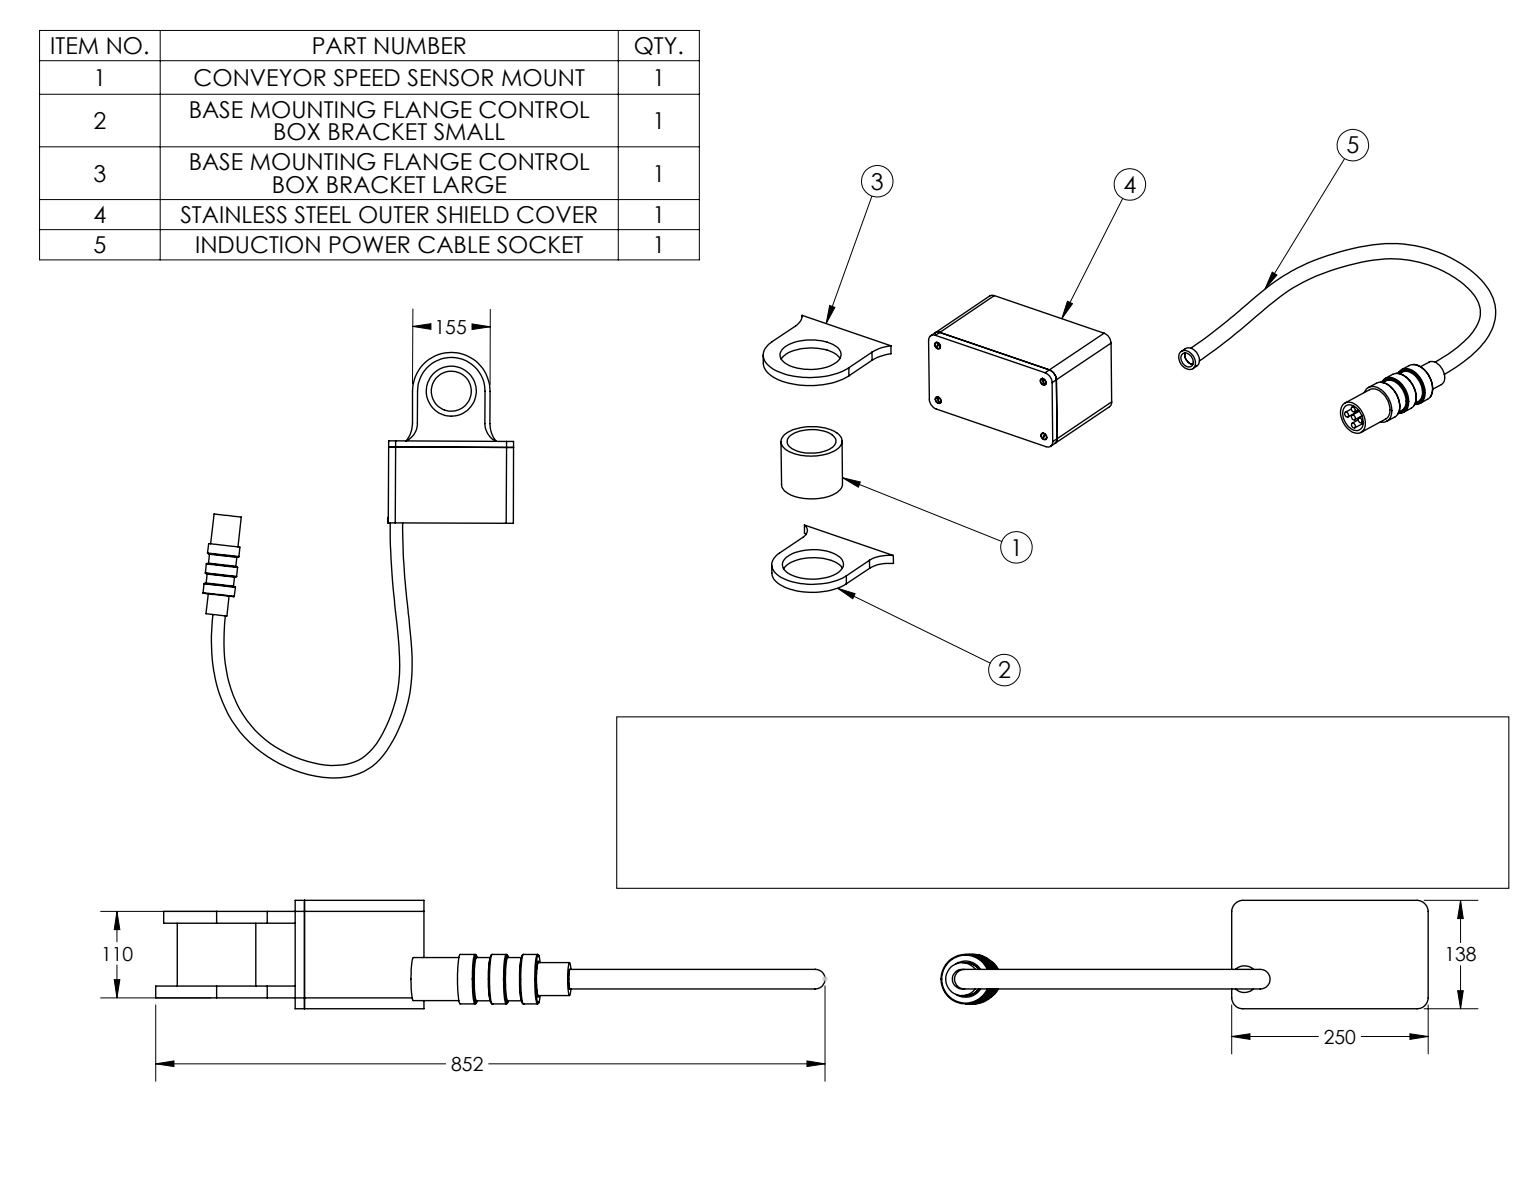
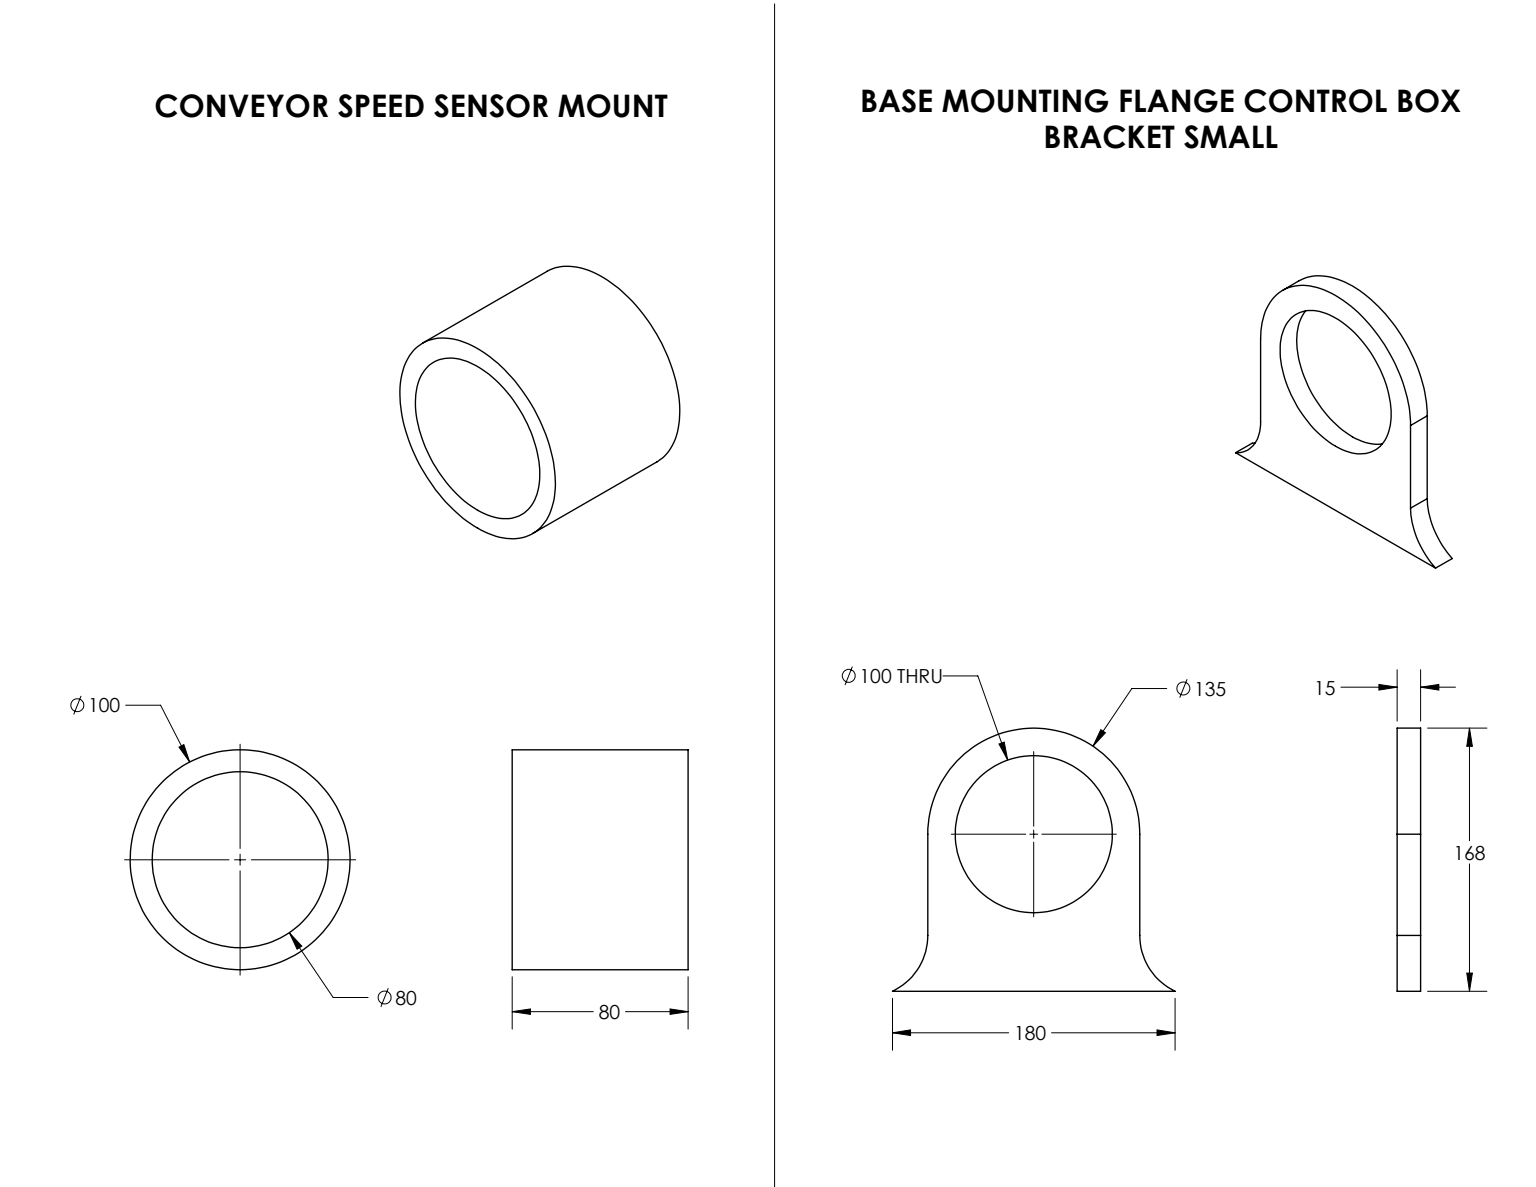
ISO-10303-21;
HEADER;
FILE_DESCRIPTION (('STEP AP214'),
    '1' );
FILE_NAME ('MAT-023',
    '2026-10-28T18:30:06',
    ( '' ),
    ( '' ),
    'SwSTEP 2.0',
    'SolidWorks 2024',
    '' );
FILE_SCHEMA (( 'AUTOMOTIVE_DESIGN' ));
ENDSEC;

DATA;
#1 = CARTESIAN_POINT ( 'NONE',  ( -382.0077566144223624, 5.421010862429173848E-17, 175.3290427019271078 ) ) ;
#2 = ORIENTED_EDGE ( 'NONE', *, *, #5398, .F. ) ;
#3 = APPLICATION_CONTEXT ( 'automotive_design' ) ;
#4 = DIRECTION ( 'NONE',  ( 5.551115123125772841E-17, -1.848892746611743135E-31, -1.000000000000000000 ) ) ;
#5 = DIRECTION ( 'NONE',  ( -0.9955873536034884896, 5.465719896581968711E-31, -0.09383933793885443353 ) ) ;
#6 = CARTESIAN_POINT ( 'NONE',  ( -84.02857808274397655, 98.45434506795682239, 152.0000000000000853 ) ) ;
#7 = DIRECTION ( 'NONE',  ( -0.000000000000000000, -1.000000000000000000, -0.000000000000000000 ) ) ;
#8 = VERTEX_POINT ( 'NONE', #1404 ) ;
#9 = ORIENTED_EDGE ( 'NONE', *, *, #3496, .F. ) ;
#10 = DIRECTION ( 'NONE',  ( 0.4205749795070160557, -0.9072577839912276954, -5.551115123125780853E-17 ) ) ;
#11 = CARTESIAN_POINT ( 'NONE',  ( 0.000000000000000000, 0.000000000000000000, 0.000000000000000000 ) ) ;
#12 = DIRECTION ( 'NONE',  ( -0.09383933793885568253, 2.673190762809473730E-31, 0.9955873536034882676 ) ) ;
#13 = EDGE_CURVE ( 'NONE', #832, #1072, #4200, .T. ) ;
#14 = SURFACE_SIDE_STYLE ('',( #2418 ) ) ;
#15 = VECTOR ( 'NONE', #512, 1000.000000000000000 ) ;
#16 = CARTESIAN_POINT ( 'NONE',  ( 29.23877717791895492, 0.000000000000000000, 67.09613410133256650 ) ) ;
#17 = CARTESIAN_POINT ( 'NONE',  ( -86.97194166595129161, 3.740497495074990297E-15, 531.0655262460708173 ) ) ;
#18 = CARTESIAN_POINT ( 'NONE',  ( -367.0460729392618759, 0.000000000000000000, 268.0688838304710089 ) ) ;
#19 = AXIS2_PLACEMENT_3D ( 'NONE', #2675, #4355, #3941 ) ;
#20 = ORIENTED_EDGE ( 'NONE', *, *, #2616, .F. ) ;
#21 = VECTOR ( 'NONE', #4832, 999.9999999999998863 ) ;
#22 = ORIENTED_EDGE ( 'NONE', *, *, #960, .T. ) ;
#23 = CARTESIAN_POINT ( 'NONE',  ( -84.02857808274400497, -39.54565493204319182, -5.551115123125782702E-14 ) ) ;
#24 = CIRCLE ( 'NONE', #2310, 4.382543221487789964 ) ;
#25 = AXIS2_PLACEMENT_3D ( 'NONE', #1773, #1368, #5093 ) ;
#26 = ORIENTED_EDGE ( 'NONE', *, *, #5308, .T. ) ;
#27 = DIRECTION ( 'NONE',  ( -1.000000000000000000, 0.000000000000000000, -7.228014483236656373E-17 ) ) ;
#28 = VECTOR ( 'NONE', #1957, 1000.000000000000114 ) ;
#29 = CIRCLE ( 'NONE', #5298, 39.24395386344908587 ) ;
#30 = DIRECTION ( 'NONE',  ( 0.09383933793885537722, -2.626968444144180508E-31, -0.9955873536034883786 ) ) ;
#31 = DIRECTION ( 'NONE',  ( 0.000000000000000000, 1.000000000000000000, 0.000000000000000000 ) ) ;
#32 = DIRECTION ( 'NONE',  ( 0.09383933793885537722, -2.626968444144180508E-31, -0.9955873536034883786 ) ) ;
#33 = DIRECTION ( 'NONE',  ( 1.000000000000000000, 0.000000000000000000, 0.000000000000000000 ) ) ;
#34 = CARTESIAN_POINT ( 'NONE',  ( -346.0119820531829191, 0.000000000000000000, 118.4559012928527721 ) ) ;
#35 = CIRCLE ( 'NONE', #3119, 30.50000000000124345 ) ;
#36 = AXIS2_PLACEMENT_3D ( 'NONE', #3078, #3164, #1374 ) ;
#37 = AXIS2_PLACEMENT_3D ( 'NONE', #784, #1656, #4559 ) ;
#38 = ORIENTED_EDGE ( 'NONE', *, *, #4267, .T. ) ;
#39 = ORIENTED_EDGE ( 'NONE', *, *, #4059, .T. ) ;
#40 = EDGE_LOOP ( 'NONE', ( #5035, #3170, #2808, #3510 ) ) ;
#41 = DIRECTION ( 'NONE',  ( -1.000000000000000000, 0.000000000000000000, 0.000000000000000000 ) ) ;
#42 = AXIS2_PLACEMENT_3D ( 'NONE', #2101, #4638, #4224 ) ;
#43 = DIRECTION ( 'NONE',  ( 0.9955873536034884896, -5.462637660443545995E-31, 0.09383933793885503027 ) ) ;
#44 = CARTESIAN_POINT ( 'NONE',  ( -379.2497704504713738, 6.080251870909620328E-15, 135.4117092198481487 ) ) ;
#45 = PRODUCT_DEFINITION_SHAPE ( 'NONE', 'NONE',  #5437 ) ;
#46 = CYLINDRICAL_SURFACE ( 'NONE', #25, 6.000000000000032863 ) ;
#47 = EDGE_LOOP ( 'NONE', ( #4656, #3822, #3045, #5223 ) ) ;
#48 = DIRECTION ( 'NONE',  ( 0.09383933793885568253, -2.673190762809473730E-31, -0.9955873536034882676 ) ) ;
#49 = CARTESIAN_POINT ( 'NONE',  ( 6.585909452853061730, 3.740497495074990297E-15, 393.9228865916071527 ) ) ;
#50 = CARTESIAN_POINT ( 'NONE',  ( -74.77857808274409024, -21.54565493204320248, -26.84924240491759662 ) ) ;
#51 = ORIENTED_EDGE ( 'NONE', *, *, #5105, .T. ) ;
#52 = ORIENTED_EDGE ( 'NONE', *, *, #5333, .F. ) ;
#53 = CARTESIAN_POINT ( 'NONE',  ( -60.76122282208098824, 0.000000000000000000, 167.0961341013325523 ) ) ;
#54 = SHAPE_REPRESENTATION_RELATIONSHIP ( 'NONE' , 'NONE' ,  #825, #4179 ) ;
#55 = FACE_BOUND ( 'NONE', #4165, .T. ) ;
#56 = EDGE_CURVE ( 'NONE', #1665, #3075, #3058, .T. ) ;
#57 = EDGE_CURVE ( 'NONE', #2668, #1622, #1040, .T. ) ;
#58 = ORIENTED_EDGE ( 'NONE', *, *, #3746, .T. ) ;
#59 = PLANE ( 'NONE',  #568 ) ;
#60 = ADVANCED_FACE ( 'NONE', ( #4394, #2277 ), #4750, .F. ) ;
#61 = EDGE_CURVE ( 'NONE', #167, #979, #3936, .T. ) ;
#62 = CARTESIAN_POINT ( 'NONE',  ( -84.02857808274400497, -39.54565493204319893, -11.99999999999984368 ) ) ;
#63 = CARTESIAN_POINT ( 'NONE',  ( 11.81831109762766729, -25.00000000000000355, 46.95220429669349471 ) ) ;
#64 = SURFACE_STYLE_USAGE ( .BOTH. , #1323 ) ;
#65 = DIRECTION ( 'NONE',  ( -1.000000000000000000, 0.000000000000000000, 0.000000000000000000 ) ) ;
#66 = CARTESIAN_POINT ( 'NONE',  ( 133.9714219172562366, -21.54565493204323090, -9.999999999999841904 ) ) ;
#67 = ORIENTED_EDGE ( 'NONE', *, *, #2103, .T. ) ;
#68 = ORIENTED_EDGE ( 'NONE', *, *, #1541, .F. ) ;
#69 = ORIENTED_EDGE ( 'NONE', *, *, #2616, .T. ) ;
#70 = DIRECTION ( 'NONE',  ( 0.09383933793885537722, -2.626968444144180508E-31, -0.9955873536034883786 ) ) ;
#71 = CARTESIAN_POINT ( 'NONE',  ( -13.34676807733242754, 3.807633061153780218E-15, 36.33529372355719289 ) ) ;
#72 = CARTESIAN_POINT ( 'NONE',  ( -84.02857808274397655, 98.45434506795682239, 152.0000000000000853 ) ) ;
#73 = CARTESIAN_POINT ( 'NONE',  ( -98.02857808274420393, -25.54565493204307813, 152.0000000000001990 ) ) ;
#74 = ORIENTED_EDGE ( 'NONE', *, *, #1802, .F. ) ;
#75 = CARTESIAN_POINT ( 'NONE',  ( -299.8611223228758149, 3.740497495074990297E-15, 439.6443911606511392 ) ) ;
#76 = CARTESIAN_POINT ( 'NONE',  ( -80.59222536594943165, -24.99999999999981881, 529.1597157429057461 ) ) ;
#77 = CARTESIAN_POINT ( 'NONE',  ( -84.02857808274407603, 84.45434506795682239, -11.99999999999995559 ) ) ;
#78 = EDGE_CURVE ( 'NONE', #3915, #4669, #546, .T. ) ;
#79 = ORIENTED_EDGE ( 'NONE', *, *, #2485, .T. ) ;
#80 = ORIENTED_EDGE ( 'NONE', *, *, #160, .F. ) ;
#81 = LINE ( 'NONE', #5048, #3867 ) ;
#82 = ORIENTED_EDGE ( 'NONE', *, *, #2341, .F. ) ;
#83 = CARTESIAN_POINT ( 'NONE',  ( -30.63277980166695258, 0.000000000000000000, 527.1358351633697339 ) ) ;
#84 = ORIENTED_EDGE ( 'NONE', *, *, #1033, .T. ) ;
#85 = EDGE_CURVE ( 'NONE', #3013, #195, #2089, .T. ) ;
#86 = PLANE ( 'NONE',  #1169 ) ;
#87 = CARTESIAN_POINT ( 'NONE',  ( -198.3455225866221667, -25.00000000000003197, 518.3576047634796851 ) ) ;
#88 = CARTESIAN_POINT ( 'NONE',  ( -72.60637664584184847, 3.252606517456513302E-16, 552.9197695054128872 ) ) ;
#89 = CARTESIAN_POINT ( 'NONE',  ( 151.9714219172562935, -25.54565493204309234, -5.551115123125782702E-14 ) ) ;
#90 = ADVANCED_FACE ( 'NONE', ( #1835, #4370 ), #3525, .T. ) ;
#91 = EDGE_LOOP ( 'NONE', ( #1303, #4558, #3690, #426 ) ) ;
#92 = ORIENTED_EDGE ( 'NONE', *, *, #2910, .T. ) ;
#93 = ORIENTED_EDGE ( 'NONE', *, *, #1802, .T. ) ;
#94 = CARTESIAN_POINT ( 'NONE',  ( -328.0684036055322963, 2.759321206427281912E-15, 40.79703369235946298 ) ) ;
#95 = FACE_OUTER_BOUND ( 'NONE', #4381, .T. ) ;
#96 = DIRECTION ( 'NONE',  ( 5.551115123125772841E-17, -1.848892746611743135E-31, -1.000000000000000000 ) ) ;
#97 = CYLINDRICAL_SURFACE ( 'NONE', #5382, 27.43532828739476415 ) ;
#98 = ORIENTED_EDGE ( 'NONE', *, *, #2578, .T. ) ;
#99 = FACE_OUTER_BOUND ( 'NONE', #532, .T. ) ;
#100 = CARTESIAN_POINT ( 'NONE',  ( -16.96312831416361533, -24.99999999999981881, 463.2830513152442222 ) ) ;
#101 = DIRECTION ( 'NONE',  ( 0.09383933793885568253, -2.673190762809473730E-31, -0.9955873536034882676 ) ) ;
#102 = AXIS2_PLACEMENT_3D ( 'NONE', #3097, #2631, #4309 ) ;
#103 = ORIENTED_EDGE ( 'NONE', *, *, #5162, .T. ) ;
#104 = AXIS2_PLACEMENT_3D ( 'NONE', #682, #917, #4326 ) ;
#105 = CARTESIAN_POINT ( 'NONE',  ( 29.23877717791895492, -14.99999999999998579, 67.09613410133256650 ) ) ;
#106 = LINE ( 'NONE', #1784, #5082 ) ;
#107 =( NAMED_UNIT ( * ) PLANE_ANGLE_UNIT ( ) SI_UNIT ( $, .RADIAN. ) );
#108 = AXIS2_PLACEMENT_3D ( 'NONE', #5417, #1651, #2776 ) ;
#109 = EDGE_LOOP ( 'NONE', ( #1428, #2018, #1351, #4648 ) ) ;
#110 = CARTESIAN_POINT ( 'NONE',  ( -285.5643670724598451, 2.222614453595284090E-15, 494.2304181244439292 ) ) ;
#111 = EDGE_CURVE ( 'NONE', #1596, #1814, #592, .T. ) ;
#112 = DIRECTION ( 'NONE',  ( 5.551115123125772841E-17, -1.848892746611743135E-31, -1.000000000000000000 ) ) ;
#113 = CARTESIAN_POINT ( 'NONE',  ( -336.1069982926118769, 1.517883041479706208E-15, 349.6877309229317916 ) ) ;
#114 = AXIS2_PLACEMENT_3D ( 'NONE', #1904, #666, #4466 ) ;
#115 = CARTESIAN_POINT ( 'NONE',  ( -364.1439395362590972, 2.398458366376004494E-13, 237.2787335496881553 ) ) ;
#116 = CARTESIAN_POINT ( 'NONE',  ( 127.9714219172562224, -21.54565493204319182, -2.000000000000002220 ) ) ;
#117 = CIRCLE ( 'NONE', #1187, 31.50000000000125766 ) ;
#118 = ORIENTED_EDGE ( 'NONE', *, *, #13, .F. ) ;
#119 = ORIENTED_EDGE ( 'NONE', *, *, #3733, .F. ) ;
#120 = ORIENTED_EDGE ( 'NONE', *, *, #4299, .T. ) ;
#121 = DIRECTION ( 'NONE',  ( 0.9998833722232041143, -6.898681060795032408E-31, -0.01527226085271977431 ) ) ;
#122 = LINE ( 'NONE', #1849, #2478 ) ;
#123 = CARTESIAN_POINT ( 'NONE',  ( 29.23877717791899400, 15.00000000000001421, -10.40386589866737488 ) ) ;
#124 = MECHANICAL_DESIGN_GEOMETRIC_PRESENTATION_REPRESENTATION (  '', ( #1085 ), #3988 ) ;
#125 = AXIS2_PLACEMENT_3D ( 'NONE', #1233, #2528, #573 ) ;
#126 = AXIS2_PLACEMENT_3D ( 'NONE', #266, #1941, #351 ) ;
#127 = SURFACE_STYLE_FILL_AREA ( #3020 ) ;
#128 = ORIENTED_EDGE ( 'NONE', *, *, #2251, .T. ) ;
#129 = EDGE_CURVE ( 'NONE', #2973, #1648, #4118, .T. ) ;
#130 = EDGE_CURVE ( 'NONE', #8, #1142, #2447, .T. ) ;
#131 = AXIS2_PLACEMENT_3D ( 'NONE', #4848, #2356, #4561 ) ;
#132 = AXIS2_PLACEMENT_3D ( 'NONE', #1581, #2880, #843 ) ;
#133 = CARTESIAN_POINT ( 'NONE',  ( 136.6230329513293213, 75.92317977368846016, -10.00000000000006395 ) ) ;
#134 = CARTESIAN_POINT ( 'NONE',  ( 23.50217280487988347, -24.99999999999981881, 428.9062724124379997 ) ) ;
#135 = CARTESIAN_POINT ( 'NONE',  ( -77.37696704867106234, 84.98551036222526989, -9.999999999999953815 ) ) ;
#136 = DIRECTION ( 'NONE',  ( -0.09383933793885536334, 2.611561004589082183E-31, 0.9955873536034882676 ) ) ;
#137 = CARTESIAN_POINT ( 'NONE',  ( -49.96441683051505578, 2.222614453595284090E-15, 542.4422122871075089 ) ) ;
#138 = DIRECTION ( 'NONE',  ( 0.3430150920801929848, -4.307264849556244242E-30, 0.9393298923196350403 ) ) ;
#139 = ORIENTED_EDGE ( 'NONE', *, *, #3662, .F. ) ;
#140 = CARTESIAN_POINT ( 'NONE',  ( -334.2906958041416488, 0.000000000000000000, 430.9840019716568804 ) ) ;
#141 = EDGE_LOOP ( 'NONE', ( #309, #4866, #1878, #776 ) ) ;
#142 = FACE_OUTER_BOUND ( 'NONE', #4109, .T. ) ;
#143 = DIRECTION ( 'NONE',  ( -5.551115123125772841E-17, 1.848892746611743135E-31, 1.000000000000000000 ) ) ;
#144 = CIRCLE ( 'NONE', #4108, 28.50000000000127898 ) ;
#145 = DIRECTION ( 'NONE',  ( 5.551115123125772841E-17, -1.848892746611743135E-31, -1.000000000000000000 ) ) ;
#146 = ORIENTED_EDGE ( 'NONE', *, *, #3858, .T. ) ;
#147 = ORIENTED_EDGE ( 'NONE', *, *, #2271, .F. ) ;
#148 = CARTESIAN_POINT ( 'NONE',  ( 29.23877717791895492, -14.99999999999998579, 117.0961341013325665 ) ) ;
#149 = CARTESIAN_POINT ( 'NONE',  ( -0.8482259245422840710, 2.276824562219559311E-15, 36.14439046289818691 ) ) ;
#150 = CARTESIAN_POINT ( 'NONE',  ( 132.2270686671744500, 85.40608534173220789, -11.99999999999990052 ) ) ;
#151 =( NAMED_UNIT ( * ) PLANE_ANGLE_UNIT ( ) SI_UNIT ( $, .RADIAN. ) );
#152 = ORIENTED_EDGE ( 'NONE', *, *, #1132, .F. ) ;
#153 = VECTOR ( 'NONE', #3723, 1000.000000000000000 ) ;
#154 = CIRCLE ( 'NONE', #4288, 50.00000000000000000 ) ;
#155 = DIRECTION ( 'NONE',  ( 0.01527226085271972227, 2.095411779493299033E-31, 0.9998833722232041143 ) ) ;
#156 = EDGE_CURVE ( 'NONE', #4669, #533, #2181, .T. ) ;
#157 = CARTESIAN_POINT ( 'NONE',  ( -57.28677601057306390, -24.99999999999981881, 546.4981013186294376 ) ) ;
#158 = CARTESIAN_POINT ( 'NONE',  ( -314.5571410767332736, 5.421010862426289575E-17, 120.4162530843239978 ) ) ;
#159 = EDGE_CURVE ( 'NONE', #2587, #907, #154, .T. ) ;
#160 = EDGE_CURVE ( 'NONE', #4568, #5281, #4983, .T. ) ;
#161 = ADVANCED_FACE ( 'NONE', ( #1208 ), #3224, .T. ) ;
#162 = EDGE_LOOP ( 'NONE', ( #316, #3364, #1642, #4137 ) ) ;
#163 = AXIS2_PLACEMENT_3D ( 'NONE', #847, #4231, #4697 ) ;
#164 = CARTESIAN_POINT ( 'NONE',  ( -364.1439395362591540, 2.222614453595284090E-15, 237.2787335496894343 ) ) ;
#165 =( NAMED_UNIT ( * ) SI_UNIT ( $, .STERADIAN. ) SOLID_ANGLE_UNIT ( ) );
#166 = EDGE_CURVE ( 'NONE', #533, #4705, #424, .T. ) ;
#167 = VERTEX_POINT ( 'NONE', #1947 ) ;
#168 = CARTESIAN_POINT ( 'NONE',  ( -207.8397519515728504, 5.421010862427522170E-17, 541.5412455041541762 ) ) ;
#169 = EDGE_LOOP ( 'NONE', ( #2313, #1592, #1135, #4605 ) ) ;
#170 = CARTESIAN_POINT ( 'NONE',  ( -84.02857808274403340, 98.45434506795682239, -12.00000000000001066 ) ) ;
#171 = DIRECTION ( 'NONE',  ( -0.9955873536034882676, 5.273458392682099492E-31, -0.09383933793885600172 ) ) ;
#172 = EDGE_LOOP ( 'NONE', ( #3037, #3349, #934, #4546, #4818, #515 ) ) ;
#173 = ORIENTED_EDGE ( 'NONE', *, *, #2818, .F. ) ;
#174 = FACE_BOUND ( 'NONE', #3528, .T. ) ;
#175 = CARTESIAN_POINT ( 'NONE',  ( -38.26122282208103798, -14.99999999999998579, 131.6034880481681171 ) ) ;
#176 = DIRECTION ( 'NONE',  ( -0.09383933793885568253, 2.673190762809473730E-31, 0.9955873536034882676 ) ) ;
#177 = CARTESIAN_POINT ( 'NONE',  ( 135.7157751673380801, 75.50260479418143689, -10.00000000000006395 ) ) ;
#178 = AXIS2_PLACEMENT_3D ( 'NONE', #5393, #3795, #1600 ) ;
#179 = VERTEX_POINT ( 'NONE', #3708 ) ;
#180 = CARTESIAN_POINT ( 'NONE',  ( -77.50517668553013095, -14.99999999999998579, 131.6034880481681171 ) ) ;
#181 = CARTESIAN_POINT ( 'NONE',  ( 18.31346110193259946, -24.99999999999981881, 444.2932575970297648 ) ) ;
#182 = DIRECTION ( 'NONE',  ( 5.551115123125772841E-17, -1.848892746611743135E-31, -1.000000000000000000 ) ) ;
#183 = ADVANCED_FACE ( 'NONE', ( #2387 ), #4883, .T. ) ;
#184 = DIRECTION ( 'NONE',  ( 0.000000000000000000, -1.000000000000000000, 0.000000000000000000 ) ) ;
#185 = DIRECTION ( 'NONE',  ( -5.551115123125785167E-17, 0.000000000000000000, -1.000000000000000000 ) ) ;
#186 = CARTESIAN_POINT ( 'NONE',  ( 29.77542608467487995, 25.00000000000000355, 249.2409987768023711 ) ) ;
#187 = DIRECTION ( 'NONE',  ( 0.000000000000000000, 0.000000000000000000, 1.000000000000000000 ) ) ;
#188 = EDGE_LOOP ( 'NONE', ( #20, #5360, #4784, #93 ) ) ;
#189 = CARTESIAN_POINT ( 'NONE',  ( 34.60640066538617532, 25.00000000000018474, 295.6817845355782879 ) ) ;
#190 = ORIENTED_EDGE ( 'NONE', *, *, #2199, .F. ) ;
#191 = CIRCLE ( 'NONE', #2391, 40.00000000000000000 ) ;
#192 = CYLINDRICAL_SURFACE ( 'NONE', #816, 5.250000000000018652 ) ;
#193 = DIRECTION ( 'NONE',  ( -0.09383933793885568253, 2.673190762809473730E-31, 0.9955873536034882676 ) ) ;
#194 = AXIS2_PLACEMENT_3D ( 'NONE', #2516, #803, #5003 ) ;
#195 = VERTEX_POINT ( 'NONE', #2772 ) ;
#196 = VECTOR ( 'NONE', #4824, 1000.000000000000000 ) ;
#197 = VECTOR ( 'NONE', #4836, 1000.000000000000000 ) ;
#198 = ORIENTED_EDGE ( 'NONE', *, *, #4878, .F. ) ;
#199 = DIRECTION ( 'NONE',  ( 0.09383933793885537722, -2.626968444144180508E-31, -0.9955873536034883786 ) ) ;
#200 = CARTESIAN_POINT ( 'NONE',  ( -98.02857808274411866, 84.45434506795672291, -12.00000000000001066 ) ) ;
#201 = CARTESIAN_POINT ( 'NONE',  ( 0.000000000000000000, 80.00000000000000000, 0.000000000000000000 ) ) ;
#202 = DIRECTION ( 'NONE',  ( 6.938893903907233308E-17, 0.000000000000000000, 1.000000000000000000 ) ) ;
#203 = PRODUCT_RELATED_PRODUCT_CATEGORY ( 'part', '', ( #1136 ) ) ;
#204 = VECTOR ( 'NONE', #2350, 1000.000000000000000 ) ;
#205 = CYLINDRICAL_SURFACE ( 'NONE', #5207, 31.50000000000125766 ) ;
#206 = ORIENTED_EDGE ( 'NONE', *, *, #2251, .F. ) ;
#207 = AXIS2_PLACEMENT_3D ( 'NONE', #2875, #1242, #4553 ) ;
#208 = CARTESIAN_POINT ( 'NONE',  ( 102.9433289385998478, 15.00000000000001421, 135.9081080810072137 ) ) ;
#209 = CIRCLE ( 'NONE', #1527, 1.000000000000000888 ) ;
#210 = CARTESIAN_POINT ( 'NONE',  ( 12.58979647763662513, -25.00000000000000355, 97.46177917735926144 ) ) ;
#211 = DIRECTION ( 'NONE',  ( 5.551115123125772841E-17, -1.848892746611743135E-31, -1.000000000000000000 ) ) ;
#212 = DIRECTION ( 'NONE',  ( -1.000000000000000000, 0.000000000000000000, -7.228014483236656373E-17 ) ) ;
#213 = VECTOR ( 'NONE', #927, 1000.000000000000000 ) ;
#214 = AXIS2_PLACEMENT_3D ( 'NONE', #4438, #1050, #3151 ) ;
#215 = ORIENTED_EDGE ( 'NONE', *, *, #4294, .F. ) ;
#216 = CARTESIAN_POINT ( 'NONE',  ( -36.58361131987991399, 0.000000000000000000, 532.6725316595221784 ) ) ;
#217 = APPLICATION_PROTOCOL_DEFINITION ( 'draft international standard', 'automotive_design', 1998, #4845 ) ;
#218 = CARTESIAN_POINT ( 'NONE',  ( 24.85474708473260108, -25.00000000000000355, 216.1905617304888665 ) ) ;
#219 = CIRCLE ( 'NONE', #2497, 5.250000000000004441 ) ;
#220 = AXIS2_PLACEMENT_3D ( 'NONE', #3082, #4782, #2665 ) ;
#221 = ORIENTED_EDGE ( 'NONE', *, *, #3158, .F. ) ;
#222 = CARTESIAN_POINT ( 'NONE',  ( 10.82492224058160879, 25.00000000000018474, 312.2165827548579387 ) ) ;
#223 = ORIENTED_EDGE ( 'NONE', *, *, #2066, .T. ) ;
#224 = EDGE_CURVE ( 'NONE', #3599, #1199, #1643, .T. ) ;
#225 = DIRECTION ( 'NONE',  ( 6.938893903907233308E-17, 0.000000000000000000, 1.000000000000000000 ) ) ;
#226 = EDGE_CURVE ( 'NONE', #1002, #2668, #2706, .T. ) ;
#227 = ADVANCED_FACE ( 'NONE', ( #4014 ), #4039, .F. ) ;
#228 = EDGE_CURVE ( 'NONE', #5171, #2162, #3633, .T. ) ;
#229 = VERTEX_POINT ( 'NONE', #3605 ) ;
#230 = ADVANCED_FACE ( 'NONE', ( #2825 ), #5293, .T. ) ;
#231 = ORIENTED_EDGE ( 'NONE', *, *, #3564, .F. ) ;
#232 = CARTESIAN_POINT ( 'NONE',  ( -86.02857808274406182, 80.45434506795689344, -2.000000000000113243 ) ) ;
#233 = PLANE ( 'NONE',  #418 ) ;
#234 = CARTESIAN_POINT ( 'NONE',  ( -84.02857808274418971, -25.54565493204318116, -5.551115123125782702E-14 ) ) ;
#235 = ADVANCED_FACE ( 'NONE', ( #2885 ), #270, .T. ) ;
#236 = CARTESIAN_POINT ( 'NONE',  ( -371.4494611792977139, 5.636683259291083957E-15, 95.96964117815871020 ) ) ;
#237 = FACE_OUTER_BOUND ( 'NONE', #3374, .T. ) ;
#238 = ORIENTED_EDGE ( 'NONE', *, *, #993, .F. ) ;
#239 = CYLINDRICAL_SURFACE ( 'NONE', #132, 5.250000000000004441 ) ;
#240 = CARTESIAN_POINT ( 'NONE',  ( -330.1866567701607096, -25.00000000000003197, 374.2973685668110306 ) ) ;
#241 = LINE ( 'NONE', #3933, #1979 ) ;
#242 = DIRECTION ( 'NONE',  ( 5.551115123125772841E-17, -1.848892746611743135E-31, -1.000000000000000000 ) ) ;
#243 = CARTESIAN_POINT ( 'NONE',  ( -66.30461487616335603, 15.00000000000001421, 161.8139267001887447 ) ) ;
#244 = EDGE_CURVE ( 'NONE', #774, #4710, #3337, .T. ) ;
#245 = CARTESIAN_POINT ( 'NONE',  ( 33.59898979596707136, 25.00000000000018474, 384.0431050523492900 ) ) ;
#246 = APPLICATION_PROTOCOL_DEFINITION ( 'draft international standard', 'automotive_design', 1998, #256 ) ;
#247 = CARTESIAN_POINT ( 'NONE',  ( 8.821273309634928950, -24.99999999999981881, 380.5076279642381110 ) ) ;
#248 = CARTESIAN_POINT ( 'NONE',  ( 11.81831109762784315, 2.222614453595197709E-15, 46.95220429669362261 ) ) ;
#249 = VERTEX_POINT ( 'NONE', #355 ) ;
#250 = CARTESIAN_POINT ( 'NONE',  ( -52.92425795465503313, 25.00000000000018474, 513.6488213284155790 ) ) ;
#251 = VERTEX_POINT ( 'NONE', #3663 ) ;
#252 = AXIS2_PLACEMENT_3D ( 'NONE', #1617, #736, #303 ) ;
#253 = CARTESIAN_POINT ( 'NONE',  ( -344.9797493358557858, 2.222614453595284090E-15, 107.5044404032143888 ) ) ;
#254 = DIRECTION ( 'NONE',  ( 5.551115123125772841E-17, -1.848892746611743135E-31, -1.000000000000000000 ) ) ;
#255 = ADVANCED_FACE ( 'NONE', ( #1536 ), #3514, .F. ) ;
#256 = APPLICATION_CONTEXT ( 'automotive_design' ) ;
#257 = ORIENTED_EDGE ( 'NONE', *, *, #966, .F. ) ;
#258 = ADVANCED_FACE ( 'NONE', ( #3277, #1121 ), #4970, .T. ) ;
#259 = EDGE_LOOP ( 'NONE', ( #3861, #904 ) ) ;
#260 = LINE ( 'NONE', #2757, #3717 ) ;
#261 = CARTESIAN_POINT ( 'NONE',  ( 137.9714219172561798, 98.45434506795687923, -5.551115123125782702E-14 ) ) ;
#262 = DIRECTION ( 'NONE',  ( -0.09383933793885568253, 2.673190762809473730E-31, 0.9955873536034882676 ) ) ;
#263 = DIRECTION ( 'NONE',  ( 1.000000000000000000, 1.261617073437686134E-16, 5.551115123125772841E-17 ) ) ;
#264 = CYLINDRICAL_SURFACE ( 'NONE', #2932, 27.50000000000126121 ) ;
#265 = VERTEX_POINT ( 'NONE', #762 ) ;
#266 = CARTESIAN_POINT ( 'NONE',  ( -84.02857808274407603, -25.54565493204318116, 152.0000000000000853 ) ) ;
#267 = DIRECTION ( 'NONE',  ( 0.000000000000000000, 0.000000000000000000, 1.000000000000000000 ) ) ;
#268 = DIRECTION ( 'NONE',  ( 0.09383933793885568253, -2.673190762809473730E-31, -0.9955873536034882676 ) ) ;
#269 = DIRECTION ( 'NONE',  ( 0.000000000000000000, 0.000000000000000000, -1.000000000000000000 ) ) ;
#270 = PLANE ( 'NONE',  #773 ) ;
#271 = CARTESIAN_POINT ( 'NONE',  ( -122.4270646331732451, 25.00000000000018474, 560.5113017241552598 ) ) ;
#272 = CONTEXT_DEPENDENT_SHAPE_REPRESENTATION ( #3254, #4906 ) ;
#273 = CARTESIAN_POINT ( 'NONE',  ( -360.7307227603797060, -24.99999999999981881, 354.4373729494859049 ) ) ;
#274 = CARTESIAN_POINT ( 'NONE',  ( -49.96441683051505578, 2.222614453595284090E-15, 542.4422122871075089 ) ) ;
#275 = EDGE_CURVE ( 'NONE', #3236, #249, #1125, .T. ) ;
#276 = VERTEX_POINT ( 'NONE', #5095 ) ;
#277 = CARTESIAN_POINT ( 'NONE',  ( -207.8397519515722252, 24.99999999999997158, 541.5412455041529256 ) ) ;
#278 = VERTEX_POINT ( 'NONE', #899 ) ;
#279 = CARTESIAN_POINT ( 'NONE',  ( -383.0971833059647338, 3.911847525938617771E-15, 176.2307907175917308 ) ) ;
#280 = CARTESIAN_POINT ( 'NONE',  ( 11.81831109762784315, 2.222614453595197709E-15, 46.95220429669362261 ) ) ;
#281 = VERTEX_POINT ( 'NONE', #1660 ) ;
#282 = UNCERTAINTY_MEASURE_WITH_UNIT (LENGTH_MEASURE( 1.000000000000000082E-05 ), #1628, 'distance_accuracy_value', 'NONE');
#283 = EDGE_LOOP ( 'NONE', ( #1020, #3448, #92, #3790 ) ) ;
#284 = CARTESIAN_POINT ( 'NONE',  ( 133.9714219172562366, 80.45434506795683660, -12.00000000000001066 ) ) ;
#285 = AXIS2_PLACEMENT_3D ( 'NONE', #400, #2072, #1734 ) ;
#286 = PLANE ( 'NONE',  #591 ) ;
#287 = PLANE ( 'NONE',  #5276 ) ;
#288 = CARTESIAN_POINT ( 'NONE',  ( -316.8209294095171913, 2.276824562219560495E-15, 101.1186672634072750 ) ) ;
#289 = DIRECTION ( 'NONE',  ( 0.000000000000000000, 0.000000000000000000, 1.000000000000000000 ) ) ;
#290 = EDGE_LOOP ( 'NONE', ( #3671, #3262, #5267, #5005 ) ) ;
#291 = AXIS2_PLACEMENT_3D ( 'NONE', #883, #526, #2643 ) ;
#292 = AXIS2_PLACEMENT_3D ( 'NONE', #5415, #4190, #801 ) ;
#293 = AXIS2_PLACEMENT_3D ( 'NONE', #771, #797, #2891 ) ;
#294 = CYLINDRICAL_SURFACE ( 'NONE', #2881, 31.50000000000125766 ) ;
#295 = DIRECTION ( 'NONE',  ( 0.000000000000000000, 1.000000000000000000, 0.000000000000000000 ) ) ;
#296 = LINE ( 'NONE', #4968, #4867 ) ;
#297 = AXIS2_PLACEMENT_3D ( 'NONE', #1076, #5275, #777 ) ;
#298 = EDGE_CURVE ( 'NONE', #1751, #1002, #1747, .T. ) ;
#299 = CARTESIAN_POINT ( 'NONE',  ( 137.9714219172563219, 84.45434506795683660, 152.0000000000003126 ) ) ;
#300 = ADVANCED_FACE ( 'NONE', ( #1281 ), #3439, .T. ) ;
#301 = CIRCLE ( 'NONE', #3552, 14.00000000000002665 ) ;
#302 = AXIS2_PLACEMENT_3D ( 'NONE', #761, #354, #430 ) ;
#303 = DIRECTION ( 'NONE',  ( 1.000000000000000000, 0.000000000000000000, 0.000000000000000000 ) ) ;
#304 = CARTESIAN_POINT ( 'NONE',  ( -16.96312831416361533, 25.00000000000018474, 463.2830513152442222 ) ) ;
#305 = CARTESIAN_POINT ( 'NONE',  ( -174.3534642324312358, -24.99999999999981881, 552.7876087698487027 ) ) ;
#306 = DIRECTION ( 'NONE',  ( -0.09383933793885536334, 2.626968444144180070E-31, 0.9955873536034882676 ) ) ;
#307 = CIRCLE ( 'NONE', #1007, 67.50000000000001421 ) ;
#308 = AXIS2_PLACEMENT_3D ( 'NONE', #4986, #4222, #450 ) ;
#309 = ORIENTED_EDGE ( 'NONE', *, *, #61, .T. ) ;
#310 = CARTESIAN_POINT ( 'NONE',  ( 10.82492224058167984, 3.740497495074990297E-15, 312.2165827548582229 ) ) ;
#311 = PRODUCT_DEFINITION_SHAPE ( 'NONE', 'NONE',  #377 ) ;
#312 = ORIENTED_EDGE ( 'NONE', *, *, #5219, .T. ) ;
#313 = DIRECTION ( 'NONE',  ( -0.09383933793885536334, 2.626968444144180070E-31, 0.9955873536034882676 ) ) ;
#314 = CARTESIAN_POINT ( 'NONE',  ( 0.000000000000000000, 80.00000000000000000, -50.00000000000000000 ) ) ;
#315 = ORIENTED_EDGE ( 'NONE', *, *, #1838, .F. ) ;
#316 = ORIENTED_EDGE ( 'NONE', *, *, #4299, .F. ) ;
#317 = CARTESIAN_POINT ( 'NONE',  ( 132.2270686671743931, -26.49739520581860219, -11.99999999999990052 ) ) ;
#318 = DIRECTION ( 'NONE',  ( 0.09383933793885568253, -2.673190762809473730E-31, -0.9955873536034882676 ) ) ;
#319 = DIRECTION ( 'NONE',  ( -0.9955873536034883786, 5.430490990731020552E-31, -0.09383933793885548824 ) ) ;
#320 = EDGE_CURVE ( 'NONE', #4212, #3680, #2499, .T. ) ;
#321 = DIRECTION ( 'NONE',  ( -0.09383933793885537722, 2.626968444144180508E-31, 0.9955873536034883786 ) ) ;
#322 = CARTESIAN_POINT ( 'NONE',  ( -353.4921497144319460, 2.222614453595284090E-15, 38.40071206960160310 ) ) ;
#323 = ORIENTED_EDGE ( 'NONE', *, *, #228, .T. ) ;
#324 = CARTESIAN_POINT ( 'NONE',  ( -0.6802310551622114954, 2.222614453595284090E-15, 47.14310755735262859 ) ) ;
#325 = DIRECTION ( 'NONE',  ( 0.09383933793885568253, -2.673190762809473730E-31, -0.9955873536034882676 ) ) ;
#326 = CARTESIAN_POINT ( 'NONE',  ( -285.5643670724598451, 2.222614453595284090E-15, 494.2304181244439292 ) ) ;
#327 = DIRECTION ( 'NONE',  ( -0.9998833722232041143, 6.892903270961872452E-31, 0.01527226085271972227 ) ) ;
#328 = CIRCLE ( 'NONE', #4621, 12.50000000000009237 ) ;
#329 = DIRECTION ( 'NONE',  ( -1.000000000000000000, 3.759415251443877379E-31, -5.551115123125772841E-17 ) ) ;
#330 = EDGE_CURVE ( 'NONE', #4669, #1438, #1570, .T. ) ;
#331 = DIRECTION ( 'NONE',  ( 0.09383933793885568253, -2.673190762809473730E-31, -0.9955873536034882676 ) ) ;
#332 = CARTESIAN_POINT ( 'NONE',  ( -339.2542556961734590, 25.00000000000018474, 239.6247169981589309 ) ) ;
#333 = CARTESIAN_POINT ( 'NONE',  ( 31.14585677005056041, -24.99999999999981881, 398.7793066466517757 ) ) ;
#334 = EDGE_CURVE ( 'NONE', #2890, #2427, #2526, .T. ) ;
#335 = EDGE_CURVE ( 'NONE', #2651, #3875, #4642, .T. ) ;
#336 = TOROIDAL_SURFACE ( 'NONE', #766, 23.00000000000115108, 2.000000000000000000 ) ;
#337 = EDGE_LOOP ( 'NONE', ( #2365, #2394 ) ) ;
#338 = CARTESIAN_POINT ( 'NONE',  ( 6.585909452840001954, 25.00000000000018474, 393.9228865916072664 ) ) ;
#339 = VERTEX_POINT ( 'NONE', #1718 ) ;
#340 = AXIS2_PLACEMENT_3D ( 'NONE', #1650, #345, #2021 ) ;
#341 = CARTESIAN_POINT ( 'NONE',  ( -363.6733932745749485, 2.759321206427299267E-15, 99.71587303862519036 ) ) ;
#342 = VERTEX_POINT ( 'NONE', #3413 ) ;
#343 = ORIENTED_EDGE ( 'NONE', *, *, #1465, .T. ) ;
#344 = DIRECTION ( 'NONE',  ( -0.9955873536034882676, 5.484003909441392533E-31, -0.09383933793885569641 ) ) ;
#345 = DIRECTION ( 'NONE',  ( 5.551115123125772841E-17, -1.848892746611743354E-31, -1.000000000000000000 ) ) ;
#346 = DIRECTION ( 'NONE',  ( -0.9955873536034884896, 5.273458392682100368E-31, -0.09383933793885443353 ) ) ;
#347 = CYLINDRICAL_SURFACE ( 'NONE', #2595, 5.250000000000004441 ) ;
#348 = DIRECTION ( 'NONE',  ( -1.000000000000000000, 0.000000000000000000, -7.228014483236656373E-17 ) ) ;
#349 = ORIENTED_EDGE ( 'NONE', *, *, #728, .T. ) ;
#350 = ORIENTED_EDGE ( 'NONE', *, *, #320, .T. ) ;
#351 = DIRECTION ( 'NONE',  ( 1.000000000000000000, 0.000000000000000000, 0.000000000000000000 ) ) ;
#352 = LINE ( 'NONE', #5372, #902 ) ;
#353 = CARTESIAN_POINT ( 'NONE',  ( 16.14979140325228357, 2.276824562219547873E-15, 35.88476202840195839 ) ) ;
#354 = DIRECTION ( 'NONE',  ( 0.09383933793885568253, -2.673190762809473730E-31, -0.9955873536034882676 ) ) ;
#355 = CARTESIAN_POINT ( 'NONE',  ( -334.2354697480813002, 2.276824562219556945E-15, 40.21575531256979019 ) ) ;
#356 = CARTESIAN_POINT ( 'NONE',  ( -364.1439395362590403, 25.00000000000018474, 237.2787335496889227 ) ) ;
#357 = EDGE_CURVE ( 'NONE', #895, #2803, #863, .T. ) ;
#358 = CARTESIAN_POINT ( 'NONE',  ( -354.3266237013149862, 5.421010862427522170E-17, 381.2801272015580025 ) ) ;
#359 = ORIENTED_EDGE ( 'NONE', *, *, #3631, .F. ) ;
#360 = CARTESIAN_POINT ( 'NONE',  ( -52.92425795464261995, 3.794707603699265519E-15, 513.6488213284153517 ) ) ;
#361 = ORIENTED_EDGE ( 'NONE', *, *, #2818, .T. ) ;
#362 = DIRECTION ( 'NONE',  ( 0.01527226085271977431, 2.087708059715749652E-31, 0.9998833722232041143 ) ) ;
#363 = VECTOR ( 'NONE', #4645, 1000.000000000000000 ) ;
#364 = CARTESIAN_POINT ( 'NONE',  ( -74.02857808274400497, 80.45434506795689344, -12.00000000000001066 ) ) ;
#365 = EDGE_CURVE ( 'NONE', #1937, #3674, #2269, .T. ) ;
#366 = ORIENTED_EDGE ( 'NONE', *, *, #1513, .F. ) ;
#367 = DIRECTION ( 'NONE',  ( 0.000000000000000000, 0.000000000000000000, -1.000000000000000000 ) ) ;
#368 = DIRECTION ( 'NONE',  ( 0.000000000000000000, -1.000000000000000000, 0.000000000000000000 ) ) ;
#369 = DIRECTION ( 'NONE',  ( 5.551115123125772841E-17, -1.848892746611743135E-31, -1.000000000000000000 ) ) ;
#370 = CARTESIAN_POINT ( 'NONE',  ( -374.3862216308840516, 1.527175779051622645E-29, 115.7814801615950984 ) ) ;
#371 = ORIENTED_EDGE ( 'NONE', *, *, #3784, .F. ) ;
#372 = VECTOR ( 'NONE', #375, 1000.000000000000114 ) ;
#373 = EDGE_LOOP ( 'NONE', ( #2567, #146 ) ) ;
#374 = CARTESIAN_POINT ( 'NONE',  ( -344.1351952944061168, 5.421010862427522170E-17, 98.54415422078321285 ) ) ;
#375 = DIRECTION ( 'NONE',  ( -0.4205749795070158337, -0.9072577839912276954, 0.000000000000000000 ) ) ;
#376 = LINE ( 'NONE', #452, #4092 ) ;
#377 = PRODUCT_DEFINITION ( 'UNKNOWN', '', #3741, #713 ) ;
#378 = CIRCLE ( 'NONE', #1955, 2.000000000000001776 ) ;
#379 = FACE_OUTER_BOUND ( 'NONE', #2146, .T. ) ;
#380 = AXIS2_PLACEMENT_3D ( 'NONE', #3630, #3981, #212 ) ;
#381 = CARTESIAN_POINT ( 'NONE',  ( -8.629236981521737349, 1.572093150103981429E-15, 142.6115645898827893 ) ) ;
#382 = VECTOR ( 'NONE', #4088, 1000.000000000000000 ) ;
#383 = CARTESIAN_POINT ( 'NONE',  ( -80.60298687151718866, 25.00000000000018474, 555.2885198911441194 ) ) ;
#384 = CARTESIAN_POINT ( 'NONE',  ( -30.63277980166695258, 0.000000000000000000, 527.1358351633697339 ) ) ;
#385 = CIRCLE ( 'NONE', #731, 1.000000000000000888 ) ;
#386 = CIRCLE ( 'NONE', #1522, 50.00000000000000000 ) ;
#387 = ORIENTED_EDGE ( 'NONE', *, *, #567, .T. ) ;
#388 = CARTESIAN_POINT ( 'NONE',  ( -84.02857808274400497, -39.54565493204319182, -5.551115123125782702E-14 ) ) ;
#389 = VECTOR ( 'NONE', #3370, 1000.000000000000000 ) ;
#390 = AXIS2_PLACEMENT_3D ( 'NONE', #820, #4287, #2907 ) ;
#391 = DIRECTION ( 'NONE',  ( -0.09383933793885537722, 2.626968444144180508E-31, 0.9955873536034883786 ) ) ;
#392 = ORIENTED_EDGE ( 'NONE', *, *, #3263, .T. ) ;
#393 = ORIENTED_EDGE ( 'NONE', *, *, #490, .T. ) ;
#394 = CIRCLE ( 'NONE', #2942, 22.67218956682437536 ) ;
#395 = AXIS2_PLACEMENT_3D ( 'NONE', #2077, #2901, #2570 ) ;
#396 = ADVANCED_FACE ( 'NONE', ( #2658 ), #3931, .F. ) ;
#397 = DIRECTION ( 'NONE',  ( -0.9955873536034882676, 0.000000000000000000, -0.09383933793885600172 ) ) ;
#398 = DIRECTION ( 'NONE',  ( -1.000000000000000000, -1.219242865862094703E-16, 0.000000000000000000 ) ) ;
#399 = EDGE_CURVE ( 'NONE', #1903, #2695, #1029, .T. ) ;
#400 = CARTESIAN_POINT ( 'NONE',  ( 29.23877717791899755, 15.00000000000001421, 67.09613410133263756 ) ) ;
#401 = CARTESIAN_POINT ( 'NONE',  ( -344.1351952944061168, 5.421010862427522170E-17, 98.54415422078321285 ) ) ;
#402 = ADVANCED_FACE ( 'NONE', ( #4799 ), #2223, .F. ) ;
#403 = ADVANCED_FACE ( 'NONE', ( #5233 ), #4724, .T. ) ;
#404 = PRODUCT_DEFINITION_FORMATION_WITH_SPECIFIED_SOURCE ( 'ANY', '', #3007, .NOT_KNOWN. ) ;
#405 = VERTEX_POINT ( 'NONE', #133 ) ;
#406 = EDGE_LOOP ( 'NONE', ( #3376, #2068, #1234, #4289 ) ) ;
#407 = DIRECTION ( 'NONE',  ( 0.000000000000000000, 1.000000000000000000, 0.000000000000000000 ) ) ;
#408 = CYLINDRICAL_SURFACE ( 'NONE', #1858, 50.00000000000000000 ) ;
#409 = DIRECTION ( 'NONE',  ( 0.09383933793885568253, -2.673190762809473730E-31, -0.9955873536034882676 ) ) ;
#410 = CARTESIAN_POINT ( 'NONE',  ( -312.0566616799237067, 1.517883041479706208E-15, 419.2731246273846182 ) ) ;
#411 = CARTESIAN_POINT ( 'NONE',  ( -52.92425795464261995, 3.794707603699265519E-15, 513.6488213284153517 ) ) ;
#412 = DIRECTION ( 'NONE',  ( -0.4205749795070160002, 0.9072577839912275843, 5.551115123125780237E-17 ) ) ;
#413 = ORIENTED_EDGE ( 'NONE', *, *, #3394, .T. ) ;
#414 = EDGE_CURVE ( 'NONE', #1788, #4543, #3759, .T. ) ;
#415 = CARTESIAN_POINT ( 'NONE',  ( -383.0033439680259448, 3.911847525938617771E-15, 175.2352033639882620 ) ) ;
#416 = CARTESIAN_POINT ( 'NONE',  ( -334.2354697480813002, -14.95948628165117178, 40.21575531256979019 ) ) ;
#417 = ORIENTED_EDGE ( 'NONE', *, *, #5228, .F. ) ;
#418 = AXIS2_PLACEMENT_3D ( 'NONE', #3239, #1138, #2812 ) ;
#419 = CARTESIAN_POINT ( 'NONE',  ( 29.23877717791899755, 15.00000000000001421, 67.09613410133263756 ) ) ;
#420 = CARTESIAN_POINT ( 'NONE',  ( -316.6216065113882223, 2.222614453595267129E-15, 142.3191748636001250 ) ) ;
#421 = CARTESIAN_POINT ( 'NONE',  ( -84.02857808274407603, -25.54565493204318116, 152.0000000000000853 ) ) ;
#422 = EDGE_CURVE ( 'NONE', #850, #3905, #3161, .T. ) ;
#423 = CYLINDRICAL_SURFACE ( 'NONE', #3820, 40.00000000000000000 ) ;
#424 = CIRCLE ( 'NONE', #1120, 28.50000000000127542 ) ;
#425 = EDGE_LOOP ( 'NONE', ( #1381, #3302, #84, #3412 ) ) ;
#426 = ORIENTED_EDGE ( 'NONE', *, *, #330, .T. ) ;
#427 = CYLINDRICAL_SURFACE ( 'NONE', #395, 50.00000000000000000 ) ;
#428 = DIRECTION ( 'NONE',  ( 5.551115123125772841E-17, -1.848892746611743135E-31, -1.000000000000000000 ) ) ;
#429 = DIRECTION ( 'NONE',  ( 0.09383933793885568253, -2.673190762809473730E-31, -0.9955873536034882676 ) ) ;
#430 = DIRECTION ( 'NONE',  ( -0.9955873536034884896, 0.000000000000000000, -0.09383933793885443353 ) ) ;
#431 = CIRCLE ( 'NONE', #178, 4.382543221487789964 ) ;
#432 = CARTESIAN_POINT ( 'NONE',  ( -5.157059352426552223, 3.740497495074990297E-15, 435.5986320196309975 ) ) ;
#433 = CARTESIAN_POINT ( 'NONE',  ( -52.92425795463013571, -24.99999999999981881, 513.6488213284161475 ) ) ;
#434 = CARTESIAN_POINT ( 'NONE',  ( 151.9714219172563219, 84.45434506795673713, 152.0000000000001990 ) ) ;
#435 = ORIENTED_EDGE ( 'NONE', *, *, #5189, .F. ) ;
#436 = ORIENTED_EDGE ( 'NONE', *, *, #4267, .F. ) ;
#437 = DIRECTION ( 'NONE',  ( 1.000000000000000000, -3.851859888774468203E-31, 0.000000000000000000 ) ) ;
#438 = FILL_AREA_STYLE_COLOUR ( '', #5205 ) ;
#439 = ORIENTED_EDGE ( 'NONE', *, *, #3868, .F. ) ;
#440 = CARTESIAN_POINT ( 'NONE',  ( 151.9714219172562935, -25.54565493204307813, 152.0000000000001990 ) ) ;
#441 = ORIENTED_EDGE ( 'NONE', *, *, #3925, .T. ) ;
#442 = CARTESIAN_POINT ( 'NONE',  ( 29.23877717791896202, -14.99999999999998579, 17.09613410133256650 ) ) ;
#443 = CYLINDRICAL_SURFACE ( 'NONE', #292, 67.50000000000001421 ) ;
#444 = PLANE ( 'NONE',  #340 ) ;
#445 = PLANE ( 'NONE',  #3284 ) ;
#446 = DIRECTION ( 'NONE',  ( -0.09383933793885537722, 2.626968444144180508E-31, 0.9955873536034883786 ) ) ;
#447 = EDGE_LOOP ( 'NONE', ( #103, #5217, #5036, #2948 ) ) ;
#448 = ORIENTED_EDGE ( 'NONE', *, *, #1946, .T. ) ;
#449 = ORIENTED_EDGE ( 'NONE', *, *, #5015, .T. ) ;
#450 = DIRECTION ( 'NONE',  ( 1.000000000000000000, -3.759415251443877379E-31, 5.551115123125772841E-17 ) ) ;
#451 = CARTESIAN_POINT ( 'NONE',  ( 137.9714219172561513, -25.54565493204318116, -11.99999999999995559 ) ) ;
#452 = CARTESIAN_POINT ( 'NONE',  ( -373.3906342772800713, 3.367778697655401562E-15, 115.8753194995341289 ) ) ;
#453 = LINE ( 'NONE', #2135, #4250 ) ;
#454 = ORIENTED_EDGE ( 'NONE', *, *, #5175, .F. ) ;
#455 = CIRCLE ( 'NONE', #1157, 5.250000000000018652 ) ;
#456 = CARTESIAN_POINT ( 'NONE',  ( 29.23877717791900466, 15.00000000000001421, 117.0961341013325949 ) ) ;
#457 = CARTESIAN_POINT ( 'NONE',  ( -268.5984117390373171, -25.00000000000003197, 475.6392848759601293 ) ) ;
#458 = FACE_OUTER_BOUND ( 'NONE', #2128, .T. ) ;
#459 = CIRCLE ( 'NONE', #5192, 31.50000000000125766 ) ;
#460 = EDGE_CURVE ( 'NONE', #2116, #2668, #3869, .T. ) ;
#461 = ADVANCED_FACE ( 'NONE', ( #99 ), #4338, .F. ) ;
#462 = EDGE_CURVE ( 'NONE', #1438, #4705, #1389, .T. ) ;
#463 = VERTEX_POINT ( 'NONE', #4747 ) ;
#464 = VECTOR ( 'NONE', #4868, 1000.000000000000114 ) ;
#465 = VECTOR ( 'NONE', #4114, 1000.000000000000114 ) ;
#466 = CIRCLE ( 'NONE', #293, 6.000000000000032863 ) ;
#467 = VERTEX_POINT ( 'NONE', #1777 ) ;
#468 = DIRECTION ( 'NONE',  ( -1.000000000000000000, 0.000000000000000000, -5.551115123125777155E-17 ) ) ;
#469 = CARTESIAN_POINT ( 'NONE',  ( -347.8887688119603467, 2.222614453595284090E-15, 138.3676483649222178 ) ) ;
#470 = AXIS2_PLACEMENT_3D ( 'NONE', #2096, #4628, #2978 ) ;
#471 = CIRCLE ( 'NONE', #1001, 14.00000000000002665 ) ;
#472 = ORIENTED_EDGE ( 'NONE', *, *, #2175, .T. ) ;
#473 = DIRECTION ( 'NONE',  ( 5.551115123125772841E-17, -1.848892746611743135E-31, -1.000000000000000000 ) ) ;
#474 = ORIENTED_EDGE ( 'NONE', *, *, #2339, .F. ) ;
#475 = CIRCLE ( 'NONE', #1688, 30.50000000000113332 ) ;
#476 = AXIS2_PLACEMENT_3D ( 'NONE', #322, #4926, #4094 ) ;
#477 = DIRECTION ( 'NONE',  ( 0.09383933793885568253, -2.673190762809473730E-31, -0.9955873536034882676 ) ) ;
#478 = CARTESIAN_POINT ( 'NONE',  ( -330.1866567701607096, -25.00000000000003197, 374.2973685668110306 ) ) ;
#479 = DIRECTION ( 'NONE',  ( 0.000000000000000000, 0.000000000000000000, 1.000000000000000000 ) ) ;
#480 = DIRECTION ( 'NONE',  ( -0.9955873536034882676, 5.498529991225538217E-31, -0.09383933793885536334 ) ) ;
#481 = CIRCLE ( 'NONE', #740, 30.50000000000124345 ) ;
#482 = CIRCLE ( 'NONE', #1008, 50.00000000000000000 ) ;
#483 = VERTEX_POINT ( 'NONE', #931 ) ;
#484 = VERTEX_POINT ( 'NONE', #4388 ) ;
#485 = ADVANCED_FACE ( 'NONE', ( #3976 ), #336, .T. ) ;
#486 = VERTEX_POINT ( 'NONE', #4365 ) ;
#487 = CARTESIAN_POINT ( 'NONE',  ( -351.6423423295148041, 5.421010862427522170E-17, 178.1911425090623311 ) ) ;
#488 = CIRCLE ( 'NONE', #4525, 12.50000000000003197 ) ;
#489 = FACE_OUTER_BOUND ( 'NONE', #91, .T. ) ;
#490 = EDGE_CURVE ( 'NONE', #2425, #3390, #3076, .T. ) ;
#491 = DIRECTION ( 'NONE',  ( -5.551115123125772841E-17, 1.848892746611743354E-31, 1.000000000000000000 ) ) ;
#492 = ORIENTED_EDGE ( 'NONE', *, *, #4304, .T. ) ;
#493 = CARTESIAN_POINT ( 'NONE',  ( -107.0991749147294172, 1.572093150103981429E-15, 535.0680222229615310 ) ) ;
#494 = CARTESIAN_POINT ( 'NONE',  ( -39.32426838447570816, -24.99999999999981881, 499.4571537926179872 ) ) ;
#495 = DIRECTION ( 'NONE',  ( -1.000000000000000000, 0.000000000000000000, 0.000000000000000000 ) ) ;
#496 = VERTEX_POINT ( 'NONE', #3951 ) ;
#497 = EDGE_LOOP ( 'NONE', ( #1461, #2820 ) ) ;
#498 = DIRECTION ( 'NONE',  ( 1.000000000000000000, 0.000000000000000000, 0.000000000000000000 ) ) ;
#499 = EDGE_CURVE ( 'NONE', #3639, #1984, #944, .T. ) ;
#500 = ORIENTED_EDGE ( 'NONE', *, *, #5068, .F. ) ;
#501 = CARTESIAN_POINT ( 'NONE',  ( 35.78913469918393275, 25.00000000000018474, 310.6402212931347435 ) ) ;
#502 = CARTESIAN_POINT ( 'NONE',  ( -80.02857808274410445, -21.54565493204320248, -12.00000000000001066 ) ) ;
#503 = CARTESIAN_POINT ( 'NONE',  ( -152.2642418386349163, 3.740497495074990297E-15, 532.1805559224781064 ) ) ;
#504 = CARTESIAN_POINT ( 'NONE',  ( -207.8397519515728504, 5.421010862427522170E-17, 541.5412455041541762 ) ) ;
#505 = DIRECTION ( 'NONE',  ( 5.551115123125772841E-17, -1.848892746611743135E-31, -1.000000000000000000 ) ) ;
#506 = TOROIDAL_SURFACE ( 'NONE', #1909, 30.50000000000110845, 1.000000000000000000 ) ;
#507 = ORIENTED_EDGE ( 'NONE', *, *, #2250, .T. ) ;
#508 = ORIENTED_EDGE ( 'NONE', *, *, #1839, .F. ) ;
#510 = ORIENTED_EDGE ( 'NONE', *, *, #2344, .T. ) ;
#509 = VECTOR ( 'NONE', #1316, 1000.000000000000000 ) ;
#511 = DIRECTION ( 'NONE',  ( -0.9955873536034884896, 5.452307672560235798E-31, -0.09383933793885443353 ) ) ;
#512 = DIRECTION ( 'NONE',  ( 1.261617073437686134E-16, -1.000000000000000000, -1.232595164407830946E-31 ) ) ;
#513 = DIRECTION ( 'NONE',  ( -0.09383933793885568253, 2.673190762809473730E-31, 0.9955873536034882676 ) ) ;
#514 = DIRECTION ( 'NONE',  ( -0.09383933793885537722, 2.626968444144180508E-31, 0.9955873536034883786 ) ) ;
#515 = ORIENTED_EDGE ( 'NONE', *, *, #725, .T. ) ;
#516 = CARTESIAN_POINT ( 'NONE',  ( -0.8482259245422840710, 2.276824562219559311E-15, 36.14439046289818691 ) ) ;
#517 = CARTESIAN_POINT ( 'NONE',  ( -80.59222536594906217, 3.740497495074990297E-15, 529.1597157429033587 ) ) ;
#518 = PLANE ( 'NONE',  #2144 ) ;
#519 = ORIENTED_EDGE ( 'NONE', *, *, #1198, .T. ) ;
#520 = ORIENTED_EDGE ( 'NONE', *, *, #1534, .F. ) ;
#521 = DIRECTION ( 'NONE',  ( -0.09383933793885536334, 2.611561004589082183E-31, 0.9955873536034882676 ) ) ;
#522 = SHAPE_REPRESENTATION_RELATIONSHIP ( 'NONE' , 'NONE' ,  #4024, #2470 ) ;
#523 = ORIENTED_EDGE ( 'NONE', *, *, #365, .T. ) ;
#524 = CARTESIAN_POINT ( 'NONE',  ( 33.59898979596731294, 5.421010862427522170E-17, 384.0431050523496310 ) ) ;
#525 = EDGE_LOOP ( 'NONE', ( #1580, #4189, #4442, #82 ) ) ;
#526 = DIRECTION ( 'NONE',  ( 0.09383933793885568253, -2.673190762809473730E-31, -0.9955873536034882676 ) ) ;
#527 = CARTESIAN_POINT ( 'NONE',  ( -342.0170653153610374, -24.99999999999981881, 268.9367132353194734 ) ) ;
#528 = CARTESIAN_POINT ( 'NONE',  ( -360.7307227603793649, 2.222614453595284090E-15, 354.4373729494858480 ) ) ;
#529 = CARTESIAN_POINT ( 'NONE',  ( 29.23877717791899755, 15.00000000000001421, 67.09613410133263756 ) ) ;
#530 = EDGE_CURVE ( 'NONE', #606, #5098, #1451, .T. ) ;
#531 = EDGE_CURVE ( 'NONE', #2111, #5400, #1371, .T. ) ;
#532 = EDGE_LOOP ( 'NONE', ( #58, #3431, #3991, #3373 ) ) ;
#533 = VERTEX_POINT ( 'NONE', #4725 ) ;
#534 = VERTEX_POINT ( 'NONE', #954 ) ;
#535 = DIRECTION ( 'NONE',  ( -0.09383933793885568253, 2.673190762809473730E-31, 0.9955873536034882676 ) ) ;
#536 = DIRECTION ( 'NONE',  ( -0.9955873536034884896, 5.462637660443545995E-31, -0.09383933793885503027 ) ) ;
#537 = DIRECTION ( 'NONE',  ( 0.09383933793885537722, -2.626968444144180508E-31, -0.9955873536034883786 ) ) ;
#538 = FACE_BOUND ( 'NONE', #4829, .T. ) ;
#539 = ORIENTED_EDGE ( 'NONE', *, *, #2452, .T. ) ;
#540 = ADVANCED_FACE ( 'NONE', ( #3272 ), #4444, .T. ) ;
#541 = DIRECTION ( 'NONE',  ( -0.9955873536034882676, 5.475514420260265162E-31, -0.09383933793885552987 ) ) ;
#542 = CARTESIAN_POINT ( 'NONE',  ( 24.85474708473287109, 3.252606517456513302E-16, 216.1905617304896623 ) ) ;
#543 = LINE ( 'NONE', #1015, #833 ) ;
#544 = VECTOR ( 'NONE', #3570, 1000.000000000000000 ) ;
#545 = CIRCLE ( 'NONE', #2298, 27.50000000000126477 ) ;
#546 = LINE ( 'NONE', #3957, #5331 ) ;
#547 = CARTESIAN_POINT ( 'NONE',  ( -285.5643670724598451, 2.222614453595284090E-15, 494.2304181244439292 ) ) ;
#548 = CARTESIAN_POINT ( 'NONE',  ( 0.000000000000000000, 0.000000000000000000, 0.000000000000000000 ) ) ;
#549 = CIRCLE ( 'NONE', #4068, 31.50000000000114397 ) ;
#550 = ORIENTED_EDGE ( 'NONE', *, *, #5015, .F. ) ;
#551 = CARTESIAN_POINT ( 'NONE',  ( 18.31346110193232590, 2.222614453595284090E-15, 444.2932575970293101 ) ) ;
#552 = EDGE_LOOP ( 'NONE', ( #2201, #2575, #4436, #4481 ) ) ;
#553 = CARTESIAN_POINT ( 'NONE',  ( -376.2630083896611382, 2.222614453595299473E-15, 135.6932272336650840 ) ) ;
#554 = CARTESIAN_POINT ( 'NONE',  ( -36.58361131987991399, 0.000000000000000000, 532.6725316595221784 ) ) ;
#555 = CARTESIAN_POINT ( 'NONE',  ( 131.3198108831832087, -26.07682022631159668, -10.00000000000000888 ) ) ;
#556 = VERTEX_POINT ( 'NONE', #4820 ) ;
#557 = VERTEX_POINT ( 'NONE', #3601 ) ;
#558 = ADVANCED_FACE ( 'NONE', ( #1172 ), #294, .T. ) ;
#559 = PRESENTATION_LAYER_ASSIGNMENT (  '', '', ( #2751 ) ) ;
#560 = EDGE_CURVE ( 'NONE', #1398, #3650, #2785, .T. ) ;
#561 = ORIENTED_EDGE ( 'NONE', *, *, #3629, .F. ) ;
#562 = DIRECTION ( 'NONE',  ( 1.000000000000000000, -5.679099018122551417E-31, 0.000000000000000000 ) ) ;
#563 = ADVANCED_FACE ( 'NONE', ( #4496 ), #506, .T. ) ;
#564 = DIRECTION ( 'NONE',  ( 1.000000000000000000, -3.851859888774468203E-31, 0.000000000000000000 ) ) ;
#565 = CARTESIAN_POINT ( 'NONE',  ( 133.9714219172562366, -21.54565493204319182, -12.00000000000006573 ) ) ;
#566 = VECTOR ( 'NONE', #2317, 1000.000000000000000 ) ;
#567 = EDGE_CURVE ( 'NONE', #5400, #5147, #758, .T. ) ;
#568 = AXIS2_PLACEMENT_3D ( 'NONE', #4963, #3656, #5315 ) ;
#569 = ORIENTED_EDGE ( 'NONE', *, *, #531, .T. ) ;
#570 = VECTOR ( 'NONE', #12, 1000.000000000000000 ) ;
#571 = DIRECTION ( 'NONE',  ( 1.000000000000000000, -3.759415251443877817E-31, 5.551115123125772841E-17 ) ) ;
#572 = CARTESIAN_POINT ( 'NONE',  ( 11.81831109762787690, 2.222614453595284090E-15, 46.95220429669389262 ) ) ;
#573 = DIRECTION ( 'NONE',  ( 1.000000000000000000, 0.000000000000000000, 0.000000000000000000 ) ) ;
#574 =( GEOMETRIC_REPRESENTATION_CONTEXT ( 3 ) GLOBAL_UNCERTAINTY_ASSIGNED_CONTEXT ( ( #3923 ) ) GLOBAL_UNIT_ASSIGNED_CONTEXT ( ( #5102, #107, #4619 ) ) REPRESENTATION_CONTEXT ( 'NONE', 'WORKASPACE' ) );
#575 = DIRECTION ( 'NONE',  ( -0.9998833722232041143, 6.779273404243020281E-31, 0.01527226085271993043 ) ) ;
#576 = CARTESIAN_POINT ( 'NONE',  ( 29.77542608467492613, 2.222614453595284090E-15, 249.2409987768030533 ) ) ;
#577 = VERTEX_POINT ( 'NONE', #5347 ) ;
#578 = CARTESIAN_POINT ( 'NONE',  ( -1.533280346156948193, 25.00000000000018474, 488.4857301958397784 ) ) ;
#579 = ORIENTED_EDGE ( 'NONE', *, *, #2512, .T. ) ;
#580 = DIRECTION ( 'NONE',  ( -1.000000000000000000, 0.000000000000000000, 0.000000000000000000 ) ) ;
#581 = CARTESIAN_POINT ( 'NONE',  ( 23.50217280488020677, 5.421010862427522170E-17, 428.9062724124374881 ) ) ;
#582 = CYLINDRICAL_SURFACE ( 'NONE', #4512, 77.49999999999998579 ) ;
#583 = ORIENTED_EDGE ( 'NONE', *, *, #5188, .F. ) ;
#584 = ORIENTED_EDGE ( 'NONE', *, *, #2199, .T. ) ;
#585 = ADVANCED_FACE ( 'NONE', ( #1973 ), #4098, .F. ) ;
#586 = DIRECTION ( 'NONE',  ( -0.09383933793885568253, 2.673190762809473730E-31, 0.9955873536034882676 ) ) ;
#587 = DIRECTION ( 'NONE',  ( -0.9955873536034882676, 5.406119142139367196E-31, -0.09383933793885596009 ) ) ;
#588 = DIRECTION ( 'NONE',  ( 0.09383933793885537722, -2.626968444144180508E-31, -0.9955873536034883786 ) ) ;
#589 = DIRECTION ( 'NONE',  ( -0.09383933793885537722, 2.611561004589082621E-31, 0.9955873536034883786 ) ) ;
#590 = ORIENTED_EDGE ( 'NONE', *, *, #226, .F. ) ;
#591 = AXIS2_PLACEMENT_3D ( 'NONE', #1966, #2725, #5312 ) ;
#592 = CIRCLE ( 'NONE', #3506, 30.50000000000113332 ) ;
#593 = CARTESIAN_POINT ( 'NONE',  ( -80.02857808274401918, 80.45434506795689344, -2.000000000000112799 ) ) ;
#594 = CARTESIAN_POINT ( 'NONE',  ( -336.1069982926114221, -24.99999999999981881, 349.6877309229307684 ) ) ;
#595 = DIRECTION ( 'NONE',  ( 5.551115123125772841E-17, -1.848892746611743135E-31, -1.000000000000000000 ) ) ;
#596 = CARTESIAN_POINT ( 'NONE',  ( -338.5986743560152377, 14.95948628165116823, 39.80450035817695209 ) ) ;
#597 = DIRECTION ( 'NONE',  ( 0.05689159511111528678, 0.000000000000000000, -0.9983803615885644689 ) ) ;
#598 = CARTESIAN_POINT ( 'NONE',  ( -174.3534642324304116, 5.421010862427522170E-17, 552.7876087698471110 ) ) ;
#599 = DIRECTION ( 'NONE',  ( 0.000000000000000000, 0.000000000000000000, 1.000000000000000000 ) ) ;
#600 = ORIENTED_EDGE ( 'NONE', *, *, #966, .T. ) ;
#601 = CARTESIAN_POINT ( 'NONE',  ( -80.60298687151718866, 25.00000000000018474, 555.2885198911441194 ) ) ;
#602 = ORIENTED_EDGE ( 'NONE', *, *, #2737, .T. ) ;
#603 = CARTESIAN_POINT ( 'NONE',  ( 29.23877717791896202, 0.000000000000000000, 17.09613410133256650 ) ) ;
#604 = DIRECTION ( 'NONE',  ( -4.476705744456277327E-17, 0.000000000000000000, -1.000000000000000000 ) ) ;
#605 = EDGE_LOOP ( 'NONE', ( #4984, #2778, #4803, #4779 ) ) ;
#606 = VERTEX_POINT ( 'NONE', #3188 ) ;
#607 = FACE_OUTER_BOUND ( 'NONE', #162, .T. ) ;
#608 = CARTESIAN_POINT ( 'NONE',  ( 29.23877717791899755, 15.00000000000001421, 67.09613410133263756 ) ) ;
#609 = CARTESIAN_POINT ( 'NONE',  ( -80.02857808274401918, 80.45434506795689344, -2.000000000000112799 ) ) ;
#610 = DIRECTION ( 'NONE',  ( 0.000000000000000000, 1.000000000000000000, 0.000000000000000000 ) ) ;
#611 = EDGE_LOOP ( 'NONE', ( #3586, #3264, #2074, #924 ) ) ;
#612 = CIRCLE ( 'NONE', #1585, 12.50000000000008704 ) ;
#613 = DIRECTION ( 'NONE',  ( -0.9955873536034882676, 5.502656983963321189E-31, -0.09383933793885568253 ) ) ;
#614 = CARTESIAN_POINT ( 'NONE',  ( -364.1439395362590403, -24.99999999999981881, 237.2787335496889227 ) ) ;
#615 = DIRECTION ( 'NONE',  ( -1.000000000000000000, -1.219242865862094703E-16, 0.000000000000000000 ) ) ;
#616 = DIRECTION ( 'NONE',  ( -0.09383933793885568253, 2.673190762809473730E-31, 0.9955873536034882676 ) ) ;
#617 = EDGE_CURVE ( 'NONE', #3157, #2425, #2058, .T. ) ;
#618 = EDGE_CURVE ( 'NONE', #2650, #994, #2027, .T. ) ;
#619 = DIRECTION ( 'NONE',  ( 1.000000000000000000, 0.000000000000000000, 5.551115123125771609E-17 ) ) ;
#620 = DIRECTION ( 'NONE',  ( -0.09383933793885536334, 2.626968444144180070E-31, 0.9955873536034882676 ) ) ;
#621 = PRODUCT_CONTEXT ( 'NONE', #2615, 'mechanical' ) ;
#622 = CARTESIAN_POINT ( 'NONE',  ( -16.96312831416361533, -24.99999999999981881, 463.2830513152442222 ) ) ;
#623 = ADVANCED_FACE ( 'NONE', ( #727, #3246 ), #3625, .T. ) ;
#624 = ADVANCED_FACE ( 'NONE', ( #4473 ), #4879, .F. ) ;
#625 = ORIENTED_EDGE ( 'NONE', *, *, #460, .F. ) ;
#626 = CARTESIAN_POINT ( 'NONE',  ( -249.5207023207449879, 24.99999999999997158, 491.2832465756976035 ) ) ;
#627 = ORIENTED_EDGE ( 'NONE', *, *, #3002, .F. ) ;
#628 = AXIS2_PLACEMENT_3D ( 'NONE', #1117, #1975, #759 ) ;
#629 = CARTESIAN_POINT ( 'NONE',  ( -319.4206898963205958, 5.712857831165392007E-15, 140.0464821425766786 ) ) ;
#630 = CARTESIAN_POINT ( 'NONE',  ( -77.37696704867106234, 84.98551036222526989, -9.999999999999953815 ) ) ;
#631 = CIRCLE ( 'NONE', #2568, 4.382543221487789076 ) ;
#632 = APPLICATION_CONTEXT ( 'automotive_design' ) ;
#633 = ORIENTED_EDGE ( 'NONE', *, *, #2013, .T. ) ;
#634 = AXIS2_PLACEMENT_3D ( 'NONE', #3604, #616, #3137 ) ;
#635 = CIRCLE ( 'NONE', #114, 1.000000000000000888 ) ;
#636 = ORIENTED_EDGE ( 'NONE', *, *, #160, .T. ) ;
#637 = DIRECTION ( 'NONE',  ( -0.9955873536034882676, 5.498835694391114214E-31, -0.09383933793885514130 ) ) ;
#638 = FACE_BOUND ( 'NONE', #3051, .T. ) ;
#639 = CYLINDRICAL_SURFACE ( 'NONE', #5014, 4.382543221487789964 ) ;
#640 = DIRECTION ( 'NONE',  ( -0.09383933793885537722, 2.611561004589082621E-31, 0.9955873536034883786 ) ) ;
#641 = AXIS2_PLACEMENT_3D ( 'NONE', #2055, #3740, #4584 ) ;
#642 = FILL_AREA_STYLE_COLOUR ( '', #3208 ) ;
#643 = ORIENTED_EDGE ( 'NONE', *, *, #2742, .F. ) ;
#644 = EDGE_CURVE ( 'NONE', #2687, #4195, #1144, .T. ) ;
#645 = FACE_OUTER_BOUND ( 'NONE', #5047, .T. ) ;
#646 = CIRCLE ( 'NONE', #3297, 30.50000000000124345 ) ;
#647 = DIRECTION ( 'NONE',  ( -0.09383933793885568253, 2.673190762809473730E-31, 0.9955873536034882676 ) ) ;
#648 = AXIS2_PLACEMENT_3D ( 'NONE', #4556, #2819, #2024 ) ;
#649 = CARTESIAN_POINT ( 'NONE',  ( -1.533280346156490337, 2.222614453595284090E-15, 488.4857301958385278 ) ) ;
#650 = CARTESIAN_POINT ( 'NONE',  ( 137.9714219172562082, 98.45434506795683660, 152.0000000000003126 ) ) ;
#651 = FACE_OUTER_BOUND ( 'NONE', #1633, .T. ) ;
#652 = AXIS2_PLACEMENT_3D ( 'NONE', #2525, #3352, #4202 ) ;
#653 = AXIS2_PLACEMENT_3D ( 'NONE', #3593, #2347, #4054 ) ;
#654 = ORIENTED_EDGE ( 'NONE', *, *, #4717, .T. ) ;
#655 = CARTESIAN_POINT ( 'NONE',  ( 24.85474708473260108, 25.00000000000000355, 216.1905617304888665 ) ) ;
#656 = APPLICATION_PROTOCOL_DEFINITION ( 'draft international standard', 'automotive_design', 1998, #5411 ) ;
#657 = CARTESIAN_POINT ( 'NONE',  ( -68.63039925413373510, -24.99999999999981881, 524.1455590405155363 ) ) ;
#658 = ADVANCED_FACE ( 'NONE', ( #2822 ), #2354, .T. ) ;
#659 = ORIENTED_EDGE ( 'NONE', *, *, #1753, .F. ) ;
#660 = CARTESIAN_POINT ( 'NONE',  ( -68.63039925413373510, 25.00000000000018474, 524.1455590405155363 ) ) ;
#661 = EDGE_LOOP ( 'NONE', ( #2351, #223 ) ) ;
#662 = DIRECTION ( 'NONE',  ( 5.551115123125772841E-17, -1.848892746611743135E-31, -1.000000000000000000 ) ) ;
#663 = DIRECTION ( 'NONE',  ( 0.000000000000000000, -1.000000000000000000, -0.000000000000000000 ) ) ;
#664 = VERTEX_POINT ( 'NONE', #4035 ) ;
#665 = EDGE_LOOP ( 'NONE', ( #4208, #1745, #2026, #1244 ) ) ;
#666 = DIRECTION ( 'NONE',  ( -1.219242865862094703E-16, 1.000000000000000000, -1.149200448409289593E-17 ) ) ;
#667 = CARTESIAN_POINT ( 'NONE',  ( -85.27857808274403340, 80.45434506795689344, -2.000000000000113243 ) ) ;
#668 = DIRECTION ( 'NONE',  ( -0.09383933793885568253, 2.673190762809473730E-31, 0.9955873536034882676 ) ) ;
#669 = LINE ( 'NONE', #3700, #1684 ) ;
#670 = DIRECTION ( 'NONE',  ( 5.551115123125772841E-17, -1.848892746611743135E-31, -1.000000000000000000 ) ) ;
#671 = ORIENTED_EDGE ( 'NONE', *, *, #3189, .F. ) ;
#672 = DIRECTION ( 'NONE',  ( 5.551115123125772841E-17, -1.848892746611743135E-31, -1.000000000000000000 ) ) ;
#673 = CARTESIAN_POINT ( 'NONE',  ( -156.9923520473269321, 0.000000000000000000, 556.8176423728721147 ) ) ;
#674 = DIRECTION ( 'NONE',  ( 0.000000000000000000, 0.000000000000000000, 1.000000000000000000 ) ) ;
#675 = ADVANCED_FACE ( 'NONE', ( #1609 ), #834, .T. ) ;
#676 = CARTESIAN_POINT ( 'NONE',  ( -340.0535087002904220, 2.276824562219573511E-15, 101.9421712359864500 ) ) ;
#677 = DIRECTION ( 'NONE',  ( 0.9955873536034882676, -5.273458392682099492E-31, 0.09383933793885600172 ) ) ;
#678 = CARTESIAN_POINT ( 'NONE',  ( 9.699276322990584731, 1.572093150103981429E-15, 297.8714164406039799 ) ) ;
#679 = ITEM_DEFINED_TRANSFORMATION ( 'NONE', 'NONE', #2597,  #2926 ) ;
#680 = CARTESIAN_POINT ( 'NONE',  ( -156.9923520473274721, -24.99999999999981881, 556.8176423728723421 ) ) ;
#681 = ADVANCED_FACE ( 'NONE', ( #2326 ), #239, .T. ) ;
#682 = CARTESIAN_POINT ( 'NONE',  ( -321.3707673825458642, 3.789382846023848702E-15, 182.0488296698010231 ) ) ;
#683 = ORIENTED_EDGE ( 'NONE', *, *, #3784, .T. ) ;
#684 = CARTESIAN_POINT ( 'NONE',  ( -121.8424039467700055, 25.00000000000018474, 535.4314447305361000 ) ) ;
#685 = EDGE_LOOP ( 'NONE', ( #5159, #4471 ) ) ;
#686 = PLANE ( 'NONE',  #989 ) ;
#687 = CARTESIAN_POINT ( 'NONE',  ( -0.8482259245422840710, 2.276824562219559311E-15, 36.14439046289818691 ) ) ;
#688 = ORIENTED_EDGE ( 'NONE', *, *, #4703, .T. ) ;
#689 = VERTEX_POINT ( 'NONE', #2165 ) ;
#690 = CARTESIAN_POINT ( 'NONE',  ( -346.0119820531829191, 0.000000000000000000, 118.4559012928527721 ) ) ;
#691 = LINE ( 'NONE', #2788, #5061 ) ;
#692 = ADVANCED_FACE ( 'NONE', ( #3776 ), #427, .T. ) ;
#693 = DIRECTION ( 'NONE',  ( 0.09383933793885568253, -2.673190762809473730E-31, -0.9955873536034882676 ) ) ;
#694 = CYLINDRICAL_SURFACE ( 'NONE', #1175, 27.50000000000126477 ) ;
#695 = EDGE_CURVE ( 'NONE', #4705, #533, #4086, .T. ) ;
#696 = CARTESIAN_POINT ( 'NONE',  ( -351.6423423295148041, 5.421010862427522170E-17, 178.1911425090623311 ) ) ;
#697 = VERTEX_POINT ( 'NONE', #2984 ) ;
#698 = DIRECTION ( 'NONE',  ( 5.551115123125772841E-17, -1.848892746611743135E-31, -1.000000000000000000 ) ) ;
#699 = DIRECTION ( 'NONE',  ( -0.9955873536034882676, 5.452307672560243681E-31, -0.09383933793885551600 ) ) ;
#700 = CARTESIAN_POINT ( 'NONE',  ( -349.1289451064980085, 2.222614453595281723E-15, 38.81196702399444121 ) ) ;
#701 = CARTESIAN_POINT ( 'NONE',  ( -378.2541830968680188, 2.222614453595300261E-15, 135.5055485577871934 ) ) ;
#702 = DIRECTION ( 'NONE',  ( 0.000000000000000000, 1.000000000000000000, 0.000000000000000000 ) ) ;
#703 = CARTESIAN_POINT ( 'NONE',  ( -360.7307227603797060, 25.00000000000018474, 354.4373729494859049 ) ) ;
#704 = CARTESIAN_POINT ( 'NONE',  ( -49.96441683051505578, 2.222614453595284090E-15, 542.4422122871075089 ) ) ;
#705 = CARTESIAN_POINT ( 'NONE',  ( -332.6117946626184221, -1.154691298157368797E-29, 200.0735156778482917 ) ) ;
#706 = EDGE_LOOP ( 'NONE', ( #2402, #1700, #643, #922 ) ) ;
#707 = CARTESIAN_POINT ( 'NONE',  ( -8.629236981521737349, 1.572093150103981429E-15, 142.6115645898827893 ) ) ;
#708 = EDGE_LOOP ( 'NONE', ( #3884, #2629, #2702, #889 ) ) ;
#709 = CARTESIAN_POINT ( 'NONE',  ( -344.9797493358557858, 2.222614453595284090E-15, 107.5044404032143888 ) ) ;
#710 = LINE ( 'NONE', #630, #2231 ) ;
#711 = AXIS2_PLACEMENT_3D ( 'NONE', #1713, #2130, #4280 ) ;
#712 = ORIENTED_EDGE ( 'NONE', *, *, #3398, .F. ) ;
#713 = PRODUCT_DEFINITION_CONTEXT ( 'detailed design', #2438, 'design' ) ;
#714 = EDGE_LOOP ( 'NONE', ( #3323, #3873, #822, #4259 ) ) ;
#715 = CIRCLE ( 'NONE', #1161, 56.63911695420845405 ) ;
#716 = DIRECTION ( 'NONE',  ( -1.000000000000000000, 0.000000000000000000, -7.228014483236656373E-17 ) ) ;
#717 = DIRECTION ( 'NONE',  ( -0.9955873536034882676, 5.502656983963321189E-31, -0.09383933793885573804 ) ) ;
#718 = DIRECTION ( 'NONE',  ( -0.09383933793885568253, 2.673190762809473730E-31, 0.9955873536034882676 ) ) ;
#719 = FACE_BOUND ( 'NONE', #4120, .T. ) ;
#720 = EDGE_CURVE ( 'NONE', #1930, #1984, #2928, .T. ) ;
#721 = CARTESIAN_POINT ( 'NONE',  ( 151.9714219172563219, 84.45434506795673713, 152.0000000000001990 ) ) ;
#722 = EDGE_LOOP ( 'NONE', ( #454, #1191, #2248, #349 ) ) ;
#723 = VECTOR ( 'NONE', #4325, 1000.000000000000000 ) ;
#724 =( GEOMETRIC_REPRESENTATION_CONTEXT ( 3 ) GLOBAL_UNCERTAINTY_ASSIGNED_CONTEXT ( ( #1159 ) ) GLOBAL_UNIT_ASSIGNED_CONTEXT ( ( #1725, #3826, #3420 ) ) REPRESENTATION_CONTEXT ( 'NONE', 'WORKASPACE' ) );
#725 = EDGE_CURVE ( 'NONE', #697, #3805, #3377, .T. ) ;
#726 = SURFACE_STYLE_USAGE ( .BOTH. , #2766 ) ;
#727 = FACE_BOUND ( 'NONE', #3395, .T. ) ;
#728 = EDGE_CURVE ( 'NONE', #1738, #3769, #5299, .T. ) ;
#729 = LINE ( 'NONE', #5348, #1860 ) ;
#730 = CARTESIAN_POINT ( 'NONE',  ( -84.02857808274407603, 84.45434506795682239, -11.99999999999995559 ) ) ;
#731 = AXIS2_PLACEMENT_3D ( 'NONE', #1299, #4655, #1195 ) ;
#732 = MECHANICAL_DESIGN_GEOMETRIC_PRESENTATION_REPRESENTATION (  '', ( #2579 ), #4507 ) ;
#733 = FILL_AREA_STYLE ('',( #4203 ) ) ;
#734 = ADVANCED_FACE ( 'NONE', ( #5038 ), #4148, .F. ) ;
#735 = CIRCLE ( 'NONE', #4776, 1.000000000000000888 ) ;
#736 = DIRECTION ( 'NONE',  ( -5.551115123125772841E-17, 1.848892746611743135E-31, 1.000000000000000000 ) ) ;
#737 = CARTESIAN_POINT ( 'NONE',  ( -330.1866567701607096, 24.99999999999997158, 374.2973685668110306 ) ) ;
#738 = CARTESIAN_POINT ( 'NONE',  ( 12.58979647763672283, 2.222614453595284090E-15, 97.46177917736021357 ) ) ;
#739 = CIRCLE ( 'NONE', #5297, 5.250000000000004441 ) ;
#740 = AXIS2_PLACEMENT_3D ( 'NONE', #2001, #1202, #5261 ) ;
#741 = AXIS2_PLACEMENT_3D ( 'NONE', #4332, #535, #1365 ) ;
#742 = VERTEX_POINT ( 'NONE', #1225 ) ;
#743 = CARTESIAN_POINT ( 'NONE',  ( -268.5984117390373171, 24.99999999999997158, 475.6392848759601293 ) ) ;
#744 = VERTEX_POINT ( 'NONE', #1679 ) ;
#745 = DIRECTION ( 'NONE',  ( -0.9955873536034882676, 5.498835694391114214E-31, -0.09383933793885536334 ) ) ;
#746 = FACE_BOUND ( 'NONE', #3021, .T. ) ;
#747 = ORIENTED_EDGE ( 'NONE', *, *, #3002, .T. ) ;
#748 = ORIENTED_EDGE ( 'NONE', *, *, #2583, .F. ) ;
#749 = DIRECTION ( 'NONE',  ( -1.000000000000000000, 0.000000000000000000, -5.551115123125777155E-17 ) ) ;
#750 = CARTESIAN_POINT ( 'NONE',  ( 139.2214219172562366, -21.54565493204319182, -2.000000000000001332 ) ) ;
#751=STYLED_ITEM('',(#5444),#1308);
#752 = DIRECTION ( 'NONE',  ( -0.9955873536034882676, 5.498529991225532962E-31, -0.09383933793885514130 ) ) ;
#753 = FACE_OUTER_BOUND ( 'NONE', #4113, .T. ) ;
#754 = DIRECTION ( 'NONE',  ( -5.720779902258401340E-31, -1.000000000000000000, 2.099398147291833041E-31 ) ) ;
#755 = ORIENTED_EDGE ( 'NONE', *, *, #3729, .T. ) ;
#756 = EDGE_CURVE ( 'NONE', #1596, #3875, #4611, .T. ) ;
#757 = EDGE_LOOP ( 'NONE', ( #2810, #4398 ) ) ;
#758 = LINE ( 'NONE', #2382, #5292 ) ;
#759 = DIRECTION ( 'NONE',  ( 0.000000000000000000, 0.000000000000000000, 1.000000000000000000 ) ) ;
#760 = FACE_OUTER_BOUND ( 'NONE', #5303, .T. ) ;
#761 = CARTESIAN_POINT ( 'NONE',  ( -344.4167133082243595, 14.95948628165116823, 101.5309162815936048 ) ) ;
#762 = CARTESIAN_POINT ( 'NONE',  ( -74.77857808274401918, 80.45434506795689344, -12.00000000000001066 ) ) ;
#763 = CARTESIAN_POINT ( 'NONE',  ( -105.2090356704102447, 25.00000000000018474, 560.1816718768288865 ) ) ;
#764 = CARTESIAN_POINT ( 'NONE',  ( -334.2906958041416488, 0.000000000000000000, 430.9840019716568804 ) ) ;
#765 = EDGE_CURVE ( 'NONE', #5037, #1126, #5401, .T. ) ;
#766 = AXIS2_PLACEMENT_3D ( 'NONE', #3468, #5178, #980 ) ;
#767 = EDGE_LOOP ( 'NONE', ( #3289, #3348, #3591, #1412 ) ) ;
#768 = CARTESIAN_POINT ( 'NONE',  ( -35.15684241565247703, 1.843143693225357538E-15, 493.9702760599520275 ) ) ;
#769 = ORIENTED_EDGE ( 'NONE', *, *, #1435, .T. ) ;
#770 = VECTOR ( 'NONE', #1379, 1000.000000000000000 ) ;
#771 = CARTESIAN_POINT ( 'NONE',  ( -80.02857808274410445, -21.54565493204320248, -12.00000000000001066 ) ) ;
#772 = DIRECTION ( 'NONE',  ( -5.551115123125772841E-17, 1.848892746611743135E-31, 1.000000000000000000 ) ) ;
#773 = AXIS2_PLACEMENT_3D ( 'NONE', #3310, #5322, #2422 ) ;
#774 = VERTEX_POINT ( 'NONE', #4607 ) ;
#775 = UNCERTAINTY_MEASURE_WITH_UNIT (LENGTH_MEASURE( 1.000000000000000082E-05 ), #2148, 'distance_accuracy_value', 'NONE');
#776 = ORIENTED_EDGE ( 'NONE', *, *, #4366, .T. ) ;
#777 = DIRECTION ( 'NONE',  ( 1.000000000000000000, 0.000000000000000000, 7.228014483236656373E-17 ) ) ;
#778 = CARTESIAN_POINT ( 'NONE',  ( -347.7949294740212736, 2.222614453595284090E-15, 137.3720610113191469 ) ) ;
#779 = CARTESIAN_POINT ( 'NONE',  ( -351.6423423295148041, 5.421010862427522170E-17, 178.1911425090623311 ) ) ;
#780 = CARTESIAN_POINT ( 'NONE',  ( 151.9714219172562935, -25.54565493204307813, 152.0000000000001990 ) ) ;
#781 = DIRECTION ( 'NONE',  ( 0.9955873536034882676, -5.273458392682099492E-31, 0.09383933793885600172 ) ) ;
#782 = ORIENTED_EDGE ( 'NONE', *, *, #3083, .F. ) ;
#783 = VERTEX_POINT ( 'NONE', #3735 ) ;
#784 = CARTESIAN_POINT ( 'NONE',  ( 135.9827310413679413, -14.99999999999998579, 131.6034880481681171 ) ) ;
#785 = FACE_OUTER_BOUND ( 'NONE', #4999, .T. ) ;
#786 = DIRECTION ( 'NONE',  ( -0.09383933793885537722, 2.626968444144180508E-31, 0.9955873536034883786 ) ) ;
#787 = PRODUCT ( 'Conveyor Speed Sensor Mount', 'Conveyor Speed Sensor Mount', '', ( #3504 ) ) ;
#788 = FACE_OUTER_BOUND ( 'NONE', #2745, .T. ) ;
#789 = DIRECTION ( 'NONE',  ( -0.9955873536034882676, 5.484003909441382024E-31, -0.09383933793885569641 ) ) ;
#790 = CARTESIAN_POINT ( 'NONE',  ( -49.96441683051492078, 25.00000000000018474, 542.4422122871054626 ) ) ;
#791 = CARTESIAN_POINT ( 'NONE',  ( 24.85474708473287109, 3.252606517456513302E-16, 216.1905617304896623 ) ) ;
#792 = EDGE_CURVE ( 'NONE', #3702, #278, #5034, .T. ) ;
#793 = EDGE_LOOP ( 'NONE', ( #1954, #4146, #1989, #3668, #231, #2566, #1032, #3056 ) ) ;
#794 = EDGE_LOOP ( 'NONE', ( #68, #829, #4704, #5108 ) ) ;
#795 = EDGE_CURVE ( 'NONE', #265, #3229, #3649, .T. ) ;
#796 = EDGE_CURVE ( 'NONE', #2890, #3556, #4181, .T. ) ;
#797 = DIRECTION ( 'NONE',  ( 5.551115123125772841E-17, -1.848892746611743135E-31, -1.000000000000000000 ) ) ;
#798 = EDGE_CURVE ( 'NONE', #1142, #3875, #3838, .T. ) ;
#799 = ORIENTED_EDGE ( 'NONE', *, *, #3017, .T. ) ;
#800 = VERTEX_POINT ( 'NONE', #865 ) ;
#801 = DIRECTION ( 'NONE',  ( 0.000000000000000000, 0.000000000000000000, 1.000000000000000000 ) ) ;
#802 = DIRECTION ( 'NONE',  ( -6.938893903907233308E-17, 0.000000000000000000, -1.000000000000000000 ) ) ;
#803 = DIRECTION ( 'NONE',  ( 0.09383933793885126939, -2.549931246368698080E-31, -0.9955873536034888227 ) ) ;
#804 = DIRECTION ( 'NONE',  ( 5.551115123125772841E-17, -1.848892746611743354E-31, -1.000000000000000000 ) ) ;
#805 = AXIS2_PLACEMENT_3D ( 'NONE', #5064, #4987, #5008 ) ;
#806 = ORIENTED_EDGE ( 'NONE', *, *, #5430, .T. ) ;
#807 = AXIS2_PLACEMENT_3D ( 'NONE', #4815, #5198, #1443 ) ;
#808 = ORIENTED_EDGE ( 'NONE', *, *, #2585, .T. ) ;
#809 = DIRECTION ( 'NONE',  ( -0.9955873536034883786, 5.499036814894887477E-31, -0.09383933793885500252 ) ) ;
#810 = DIRECTION ( 'NONE',  ( 0.000000000000000000, -1.000000000000000000, 0.000000000000000000 ) ) ;
#811 = DIRECTION ( 'NONE',  ( 5.551115123125772841E-17, -1.848892746611743135E-31, -1.000000000000000000 ) ) ;
#812 = CIRCLE ( 'NONE', #2398, 14.00000000000001243 ) ;
#813 = ADVANCED_FACE ( 'NONE', ( #4252, #3350 ), #2545, .F. ) ;
#814 = CARTESIAN_POINT ( 'NONE',  ( -384.7862913888641287, 3.911847525938622504E-15, 194.1513630824538268 ) ) ;
#815 = APPLICATION_CONTEXT ( 'automotive_design' ) ;
#816 = AXIS2_PLACEMENT_3D ( 'NONE', #1900, #4808, #4021 ) ;
#817 = CARTESIAN_POINT ( 'NONE',  ( 9.699276322990584731, 1.572093150103981429E-15, 297.8714164406039799 ) ) ;
#818 = CIRCLE ( 'NONE', #906, 12.50000000000002842 ) ;
#819 = CARTESIAN_POINT ( 'NONE',  ( -48.20943979673047863, 3.740497495074990297E-15, 509.2978244404888528 ) ) ;
#820 = CARTESIAN_POINT ( 'NONE',  ( -353.5191290882918338, 0.000000000000000000, 198.1028895811323025 ) ) ;
#821 = VECTOR ( 'NONE', #1526, 1000.000000000000000 ) ;
#822 = ORIENTED_EDGE ( 'NONE', *, *, #399, .T. ) ;
#823 = EDGE_CURVE ( 'NONE', #5244, #1903, #1884, .T. ) ;
#824 = CARTESIAN_POINT ( 'NONE',  ( -344.4167133082243595, 2.222614453595284090E-15, 101.5309162815936048 ) ) ;
#825 = SHAPE_REPRESENTATION ( 'Base Mounting Flange Control Box Bracket large', ( #2926 ), #1963 ) ;
#826 = EDGE_CURVE ( 'NONE', #3068, #742, #3306, .T. ) ;
#827 = VECTOR ( 'NONE', #4315, 1000.000000000000000 ) ;
#828 = CARTESIAN_POINT ( 'NONE',  ( 0.000000000000000000, 80.00000000000000000, 0.000000000000000000 ) ) ;
#829 = ORIENTED_EDGE ( 'NONE', *, *, #2234, .F. ) ;
#830 = AXIS2_PLACEMENT_3D ( 'NONE', #4996, #4544, #4079 ) ;
#831 = AXIS2_PLACEMENT_3D ( 'NONE', #1288, #2532, #4209 ) ;
#832 = VERTEX_POINT ( 'NONE', #4659 ) ;
#833 = VECTOR ( 'NONE', #4801, 1000.000000000000000 ) ;
#834 = TOROIDAL_SURFACE ( 'NONE', #2937, 30.50000000000105516, 1.000000000000000000 ) ;
#835 = PRODUCT ( 'Base Mounting Flange Control Box Bracket large', 'Base Mounting Flange Control Box Bracket large', '', ( #4423 ) ) ;
#836 = LINE ( 'NONE', #4574, #5112 ) ;
#837 = DIRECTION ( 'NONE',  ( 0.000000000000000000, -1.000000000000000000, 0.000000000000000000 ) ) ;
#838 = CARTESIAN_POINT ( 'NONE',  ( -0.8482259245422840710, 2.276824562219559311E-15, 36.14439046289818691 ) ) ;
#839 = DIRECTION ( 'NONE',  ( 0.9955873536034882676, -5.498835694391114214E-31, 0.09383933793885514130 ) ) ;
#840 = AXIS2_PLACEMENT_3D ( 'NONE', #5215, #2279, #4372 ) ;
#841 = ORIENTED_EDGE ( 'NONE', *, *, #3959, .F. ) ;
#842 = EDGE_LOOP ( 'NONE', ( #5325, #2255 ) ) ;
#843 = DIRECTION ( 'NONE',  ( 1.000000000000000000, 0.000000000000000000, 0.000000000000000000 ) ) ;
#844 = DIRECTION ( 'NONE',  ( 0.000000000000000000, 0.000000000000000000, -1.000000000000000000 ) ) ;
#845 = DIRECTION ( 'NONE',  ( 4.476705744456277327E-17, 0.000000000000000000, 1.000000000000000000 ) ) ;
#846 = CARTESIAN_POINT ( 'NONE',  ( 137.9714219172561798, 98.45434506795689344, -5.551115123125782702E-14 ) ) ;
#847 = CARTESIAN_POINT ( 'NONE',  ( -351.5485029915759583, 2.222614453595284090E-15, 177.1955551554592603 ) ) ;
#848 = CARTESIAN_POINT ( 'NONE',  ( -13.17877320795229856, -25.00000000000000355, 47.33401081801169141 ) ) ;
#849 = CARTESIAN_POINT ( 'NONE',  ( -74.77857808274410445, -21.54565493204320248, -12.00000000000001066 ) ) ;
#850 = VERTEX_POINT ( 'NONE', #891 ) ;
#851 = DIRECTION ( 'NONE',  ( -0.09383933793885536334, 2.611561004589082183E-31, 0.9955873536034882676 ) ) ;
#852 =( LENGTH_UNIT ( ) NAMED_UNIT ( * ) SI_UNIT ( .MILLI., .METRE. ) );
#853 = ORIENTED_EDGE ( 'NONE', *, *, #4537, .F. ) ;
#854 = CIRCLE ( 'NONE', #4046, 21.00000000000012790 ) ;
#855 = CARTESIAN_POINT ( 'NONE',  ( -78.28422483266226095, 85.40608534173227895, -10.00000000000006395 ) ) ;
#856 = LINE ( 'NONE', #1649, #465 ) ;
#857 = CARTESIAN_POINT ( 'NONE',  ( -78.28422483266231779, -26.49739520581859153, -10.00000000000006395 ) ) ;
#858 = FACE_OUTER_BOUND ( 'NONE', #661, .T. ) ;
#859 = FACE_OUTER_BOUND ( 'NONE', #4770, .T. ) ;
#860 = VERTEX_POINT ( 'NONE', #4966 ) ;
#861 = VERTEX_POINT ( 'NONE', #1003 ) ;
#862 = ADVANCED_FACE ( 'NONE', ( #607 ), #3459, .T. ) ;
#863 = CIRCLE ( 'NONE', #3943, 50.00000000000000000 ) ;
#864 = VERTEX_POINT ( 'NONE', #3862 ) ;
#865 = CARTESIAN_POINT ( 'NONE',  ( 135.7157751673381370, -16.59391465826787027, -11.99999999999995559 ) ) ;
#866 = ADVANCED_FACE ( 'NONE', ( #975 ), #3946, .T. ) ;
#867 = DIRECTION ( 'NONE',  ( 0.000000000000000000, 0.000000000000000000, 1.000000000000000000 ) ) ;
#868 = CARTESIAN_POINT ( 'NONE',  ( 133.9714219172562366, -21.54565493204319182, -2.000000000000001776 ) ) ;
#869 = EDGE_CURVE ( 'NONE', #3237, #4129, #2674, .T. ) ;
#870 = CARTESIAN_POINT ( 'NONE',  ( -68.63039925413394826, 1.572093150103981429E-15, 524.1455590405157636 ) ) ;
#871 = CARTESIAN_POINT ( 'NONE',  ( -107.0991749147297014, -24.99999999999981881, 535.0680222229608489 ) ) ;
#872 = DIRECTION ( 'NONE',  ( 0.09383933793885568253, -2.673190762809473730E-31, -0.9955873536034882676 ) ) ;
#873 = PRODUCT_DEFINITION_SHAPE ( 'NONE', 'NONE',  #5435 ) ;
#874 = ORIENTED_EDGE ( 'NONE', *, *, #2540, .F. ) ;
#875 = ORIENTED_EDGE ( 'NONE', *, *, #1230, .F. ) ;
#876 = PLANE ( 'NONE',  #4144 ) ;
#877 =( NAMED_UNIT ( * ) SI_UNIT ( $, .STERADIAN. ) SOLID_ANGLE_UNIT ( ) );
#878 = CYLINDRICAL_SURFACE ( 'NONE', #2935, 5.250000000000018652 ) ;
#879 = ADVANCED_FACE ( 'NONE', ( #1442, #5088, #4742, #3047, #174, #3926 ), #3537, .T. ) ;
#880 = ORIENTED_EDGE ( 'NONE', *, *, #965, .F. ) ;
#881 = LINE ( 'NONE', #2439, #2057 ) ;
#882 = ADVANCED_FACE ( 'NONE', ( #3889 ), #3968, .F. ) ;
#883 = CARTESIAN_POINT ( 'NONE',  ( -344.1351952944073105, 5.421010862427522170E-17, 98.54415422078299969 ) ) ;
#884 = DIRECTION ( 'NONE',  ( 0.09383933793885126939, -2.549931246368698080E-31, -0.9955873536034888227 ) ) ;
#885 = CYLINDRICAL_SURFACE ( 'NONE', #4185, 50.00000000000000000 ) ;
#886 = DIRECTION ( 'NONE',  ( 5.551115123125772841E-17, -1.848892746611743135E-31, -1.000000000000000000 ) ) ;
#887 = DIRECTION ( 'NONE',  ( -1.000000000000000000, 3.759415251443877379E-31, -5.551115123125772841E-17 ) ) ;
#888 = ORIENTED_EDGE ( 'NONE', *, *, #4057, .F. ) ;
#889 = ORIENTED_EDGE ( 'NONE', *, *, #4257, .F. ) ;
#890 = ORIENTED_EDGE ( 'NONE', *, *, #5426, .F. ) ;
#891 = CARTESIAN_POINT ( 'NONE',  ( -98.02857808274411866, 84.45434506795672291, 152.0000000000001990 ) ) ;
#892 = DIRECTION ( 'NONE',  ( -1.000000000000000000, 0.000000000000000000, 0.000000000000000000 ) ) ;
#893 = CARTESIAN_POINT ( 'NONE',  ( -80.02857808274401918, 80.45434506795689344, -12.00000000000001066 ) ) ;
#894 = EDGE_CURVE ( 'NONE', #4568, #3984, #2592, .T. ) ;
#895 = VERTEX_POINT ( 'NONE', #3517 ) ;
#896 = AXIS2_PLACEMENT_3D ( 'NONE', #11, #3839, #867 ) ;
#897 = ADVANCED_FACE ( 'NONE', ( #1803 ), #5212, .T. ) ;
#898 = EDGE_CURVE ( 'NONE', #5006, #1349, #5119, .T. ) ;
#899 = CARTESIAN_POINT ( 'NONE',  ( -312.7741936558949760, 5.421010862425789758E-17, 101.5000933658572819 ) ) ;
#900 = CARTESIAN_POINT ( 'NONE',  ( -8.629236981504860182, -25.00000000000000355, 142.6115645898824198 ) ) ;
#901 = CARTESIAN_POINT ( 'NONE',  ( -374.2387848380886908, 2.625968386833892010E-15, 194.1410887772089779 ) ) ;
#902 = VECTOR ( 'NONE', #295, 1000.000000000000000 ) ;
#903 = AXIS2_PLACEMENT_3D ( 'NONE', #2789, #693, #346 ) ;
#904 = ORIENTED_EDGE ( 'NONE', *, *, #244, .T. ) ;
#905 = AXIS2_PLACEMENT_3D ( 'NONE', #4213, #4650, #2237 ) ;
#906 = AXIS2_PLACEMENT_3D ( 'NONE', #3293, #884, #2070 ) ;
#907 = VERTEX_POINT ( 'NONE', #148 ) ;
#908 = CARTESIAN_POINT ( 'NONE',  ( -344.4167133082243595, 14.95948628165116823, 101.5309162815936048 ) ) ;
#909 = CARTESIAN_POINT ( 'NONE',  ( 132.2270686671745068, 85.40608534173219368, -9.999999999999953815 ) ) ;
#910 = AXIS2_PLACEMENT_3D ( 'NONE', #5121, #513, #5150 ) ;
#911 = VERTEX_POINT ( 'NONE', #2606 ) ;
#912 = DIRECTION ( 'NONE',  ( 5.551115123125772841E-17, -1.848892746611743135E-31, -1.000000000000000000 ) ) ;
#913 = VECTOR ( 'NONE', #2782, 1000.000000000000114 ) ;
#914 = AXIS2_PLACEMENT_3D ( 'NONE', #2171, #3387, #4641 ) ;
#915 = FACE_OUTER_BOUND ( 'NONE', #3184, .T. ) ;
#916 = CARTESIAN_POINT ( 'NONE',  ( 9.699276322990401766, -24.99999999999981881, 297.8714164406044915 ) ) ;
#917 = DIRECTION ( 'NONE',  ( -1.219242865862094703E-16, 1.000000000000000000, -1.149200448409285278E-17 ) ) ;
#918 = CARTESIAN_POINT ( 'NONE',  ( 133.9714219172562366, -21.54565493204319182, -12.00000000000006573 ) ) ;
#919 = CIRCLE ( 'NONE', #2241, 5.250000000000018652 ) ;
#920 = CIRCLE ( 'NONE', #653, 5.250000000000004441 ) ;
#921 = VERTEX_POINT ( 'NONE', #5197 ) ;
#922 = ORIENTED_EDGE ( 'NONE', *, *, #4994, .F. ) ;
#923 = PRESENTATION_LAYER_ASSIGNMENT (  '', '', ( #4778 ) ) ;
#924 = ORIENTED_EDGE ( 'NONE', *, *, #5184, .F. ) ;
#925 = CARTESIAN_POINT ( 'NONE',  ( -359.3101886666408404, 0.000000000000000000, 100.1271279930180356 ) ) ;
#926 = CARTESIAN_POINT ( 'NONE',  ( -380.1309698556455601, 2.222614453595300656E-15, 155.4172956298577901 ) ) ;
#927 = DIRECTION ( 'NONE',  ( 5.551115123125772841E-17, -1.848892746611743135E-31, -1.000000000000000000 ) ) ;
#928 = PRODUCT_DEFINITION_FORMATION_WITH_SPECIFIED_SOURCE ( 'ANY', '', #787, .NOT_KNOWN. ) ;
#929 = DIRECTION ( 'NONE',  ( 0.9955873536034883786, -5.498529991225532086E-31, 0.09383933793885522456 ) ) ;
#930 = ORIENTED_EDGE ( 'NONE', *, *, #3430, .F. ) ;
#931 = CARTESIAN_POINT ( 'NONE',  ( -84.02857808274400497, -39.54565493204319182, -5.551115123125782702E-14 ) ) ;
#932 = CARTESIAN_POINT ( 'NONE',  ( -299.8611223228758149, 3.740497495074990297E-15, 439.6443911606511392 ) ) ;
#933 = CARTESIAN_POINT ( 'NONE',  ( -81.77293133282597637, 75.50260479418152215, -10.00000000000000888 ) ) ;
#934 = ORIENTED_EDGE ( 'NONE', *, *, #3288, .T. ) ;
#935 = ADVANCED_FACE ( 'NONE', ( #3434 ), #5172, .F. ) ;
#936 = VERTEX_POINT ( 'NONE', #3096 ) ;
#937 = CARTESIAN_POINT ( 'NONE',  ( 29.23877717791899400, 0.000000000000000000, -10.40386589866737488 ) ) ;
#938 = ORIENTED_EDGE ( 'NONE', *, *, #462, .F. ) ;
#939 = CARTESIAN_POINT ( 'NONE',  ( -19.78983854945498422, 2.222614453595284090E-15, 515.1268587725810448 ) ) ;
#940 = CARTESIAN_POINT ( 'NONE',  ( 6.123233995736766085E-15, 80.00000000000000000, 50.00000000000000000 ) ) ;
#941 = CARTESIAN_POINT ( 'NONE',  ( 4.992201166475765284, -24.99999999999981881, 252.6216919286950429 ) ) ;
#942 = CARTESIAN_POINT ( 'NONE',  ( -14.89480152442229688, 0.000000000000000000, 508.6517828409968729 ) ) ;
#943 = DIRECTION ( 'NONE',  ( -0.9955873536034882676, 5.452307672560245432E-31, -0.09383933793885568253 ) ) ;
#944 = CIRCLE ( 'NONE', #5153, 5.250000000000018652 ) ;
#945 = ORIENTED_EDGE ( 'NONE', *, *, #5283, .F. ) ;
#946 = ORIENTED_EDGE ( 'NONE', *, *, #4729, .T. ) ;
#947 = ORIENTED_EDGE ( 'NONE', *, *, #2735, .F. ) ;
#948 = DIRECTION ( 'NONE',  ( 0.05689159511111530065, 0.000000000000000000, -0.9983803615885645799 ) ) ;
#949 = CARTESIAN_POINT ( 'NONE',  ( -351.6423423295148041, 5.421010862427522170E-17, 178.1911425090623311 ) ) ;
#950 = CARTESIAN_POINT ( 'NONE',  ( -377.2380471327739997, 5.590393151250686046E-15, 156.6944009972769152 ) ) ;
#951 = CARTESIAN_POINT ( 'NONE',  ( -357.2727026058461206, 5.421010862427522170E-17, 237.9263837252718758 ) ) ;
#952 = ORIENTED_EDGE ( 'NONE', *, *, #826, .T. ) ;
#953 = AXIS2_PLACEMENT_3D ( 'NONE', #5351, #4856, #4103 ) ;
#954 = CARTESIAN_POINT ( 'NONE',  ( -74.02857808274400497, 80.45434506795689344, -2.000000000000112355 ) ) ;
#955 = CARTESIAN_POINT ( 'NONE',  ( -1.533280346156948193, -24.99999999999981881, 488.4857301958397784 ) ) ;
#956 = CARTESIAN_POINT ( 'NONE',  ( -80.02857808274401918, 80.45434506795689344, -2.000000000000112799 ) ) ;
#957 = DIRECTION ( 'NONE',  ( -0.01527226085271972227, -2.080004339938201146E-31, -0.9998833722232041143 ) ) ;
#958 = DIRECTION ( 'NONE',  ( -0.9955873536034884896, 0.000000000000000000, -0.09383933793885443353 ) ) ;
#959 = DIRECTION ( 'NONE',  ( 0.000000000000000000, 0.000000000000000000, 1.000000000000000000 ) ) ;
#960 = EDGE_CURVE ( 'NONE', #4918, #3848, #482, .T. ) ;
#961 = EDGE_CURVE ( 'NONE', #1937, #4307, #3014, .T. ) ;
#962 = ORIENTED_EDGE ( 'NONE', *, *, #4572, .T. ) ;
#963 = CARTESIAN_POINT ( 'NONE',  ( 24.85474708473260108, 25.00000000000000355, 216.1905617304888665 ) ) ;
#964 = VERTEX_POINT ( 'NONE', #4383 ) ;
#965 = EDGE_CURVE ( 'NONE', #3650, #1398, #1621, .T. ) ;
#966 = EDGE_CURVE ( 'NONE', #2722, #2477, #2192, .T. ) ;
#967 = FACE_OUTER_BOUND ( 'NONE', #1472, .T. ) ;
#968 = CARTESIAN_POINT ( 'NONE',  ( -312.0566616799237067, 1.517883041479706208E-15, 419.2731246273846182 ) ) ;
#969 = CARTESIAN_POINT ( 'NONE',  ( -285.5643670724598451, 2.222614453595284090E-15, 494.2304181244439292 ) ) ;
#970 = CARTESIAN_POINT ( 'NONE',  ( -323.7051989975983588, 2.222614453595284090E-15, 41.20828864675230108 ) ) ;
#971 = EDGE_CURVE ( 'NONE', #3674, #1937, #3559, .T. ) ;
#972 = ORIENTED_EDGE ( 'NONE', *, *, #3185, .F. ) ;
#973 = EDGE_LOOP ( 'NONE', ( #5370, #5420, #2966, #2980 ) ) ;
#974 = ORIENTED_EDGE ( 'NONE', *, *, #4199, .T. ) ;
#975 = FACE_OUTER_BOUND ( 'NONE', #2093, .T. ) ;
#976 = CARTESIAN_POINT ( 'NONE',  ( -98.02857808274411866, 84.45434506795672291, 152.0000000000001990 ) ) ;
#977 = CARTESIAN_POINT ( 'NONE',  ( 0.000000000000000000, 80.00000000000000000, 0.000000000000000000 ) ) ;
#978 =( NAMED_UNIT ( * ) PLANE_ANGLE_UNIT ( ) SI_UNIT ( $, .RADIAN. ) );
#979 = VERTEX_POINT ( 'NONE', #261 ) ;
#980 = DIRECTION ( 'NONE',  ( -0.9955873536034882676, 5.498529991225541720E-31, -0.09383933793885536334 ) ) ;
#981 = CARTESIAN_POINT ( 'NONE',  ( 12.58979647763672283, 2.222614453595284090E-15, 97.46177917736021357 ) ) ;
#982 = CARTESIAN_POINT ( 'NONE',  ( 133.9714219172562650, 80.45434506795682239, -9.999999999999841904 ) ) ;
#983 = EDGE_CURVE ( 'NONE', #4831, #4212, #1447, .T. ) ;
#984 = AXIS2_PLACEMENT_3D ( 'NONE', #2444, #5319, #699 ) ;
#985 = AXIS2_PLACEMENT_3D ( 'NONE', #2897, #886, #65 ) ;
#986 = DIRECTION ( 'NONE',  ( -5.551115123125772841E-17, 1.848892746611743135E-31, 1.000000000000000000 ) ) ;
#987 = CARTESIAN_POINT ( 'NONE',  ( -19.78983854945498422, 2.222614453595284090E-15, 515.1268587725810448 ) ) ;
#988 =( LENGTH_UNIT ( ) NAMED_UNIT ( * ) SI_UNIT ( .MILLI., .METRE. ) );
#989 = AXIS2_PLACEMENT_3D ( 'NONE', #1462, #4401, #3145 ) ;
#990 = VECTOR ( 'NONE', #1669, 1000.000000000000000 ) ;
#991 = ORIENTED_EDGE ( 'NONE', *, *, #1776, .T. ) ;
#992 = CARTESIAN_POINT ( 'NONE',  ( -354.3266237013149862, 5.421010862427522170E-17, 381.2801272015580025 ) ) ;
#993 = EDGE_CURVE ( 'NONE', #484, #1678, #920, .T. ) ;
#994 = VERTEX_POINT ( 'NONE', #667 ) ;
#995 = CYLINDRICAL_SURFACE ( 'NONE', #1865, 50.00000000000000000 ) ;
#996 = CIRCLE ( 'NONE', #3207, 6.000000000000032863 ) ;
#997 = CARTESIAN_POINT ( 'NONE',  ( -334.2906958041416488, 0.000000000000000000, 430.9840019716568804 ) ) ;
#998 = DIRECTION ( 'NONE',  ( 0.09383933793885568253, -2.673190762809473730E-31, -0.9955873536034882676 ) ) ;
#999 = AXIS2_PLACEMENT_3D ( 'NONE', #970, #1411, #171 ) ;
#1000 = ORIENTED_EDGE ( 'NONE', *, *, #1392, .F. ) ;
#1001 = AXIS2_PLACEMENT_3D ( 'NONE', #4562, #5404, #2498 ) ;
#1002 = VERTEX_POINT ( 'NONE', #1518 ) ;
#1003 = CARTESIAN_POINT ( 'NONE',  ( -383.8845433731994490, 1.677051647323856397E-29, 195.2407897739975624 ) ) ;
#1004 = DIRECTION ( 'NONE',  ( 0.000000000000000000, 1.000000000000000000, 0.000000000000000000 ) ) ;
#1005 = CYLINDRICAL_SURFACE ( 'NONE', #3720, 40.00000000000000000 ) ;
#1006 = VECTOR ( 'NONE', #5359, 1000.000000000000000 ) ;
#1007 = AXIS2_PLACEMENT_3D ( 'NONE', #4386, #610, #289 ) ;
#1008 = AXIS2_PLACEMENT_3D ( 'NONE', #1026, #4765, #2630 ) ;
#1009 = AXIS2_PLACEMENT_3D ( 'NONE', #4115, #368, #802 ) ;
#1010 = ORIENTED_EDGE ( 'NONE', *, *, #5425, .T. ) ;
#1011 = MECHANICAL_DESIGN_GEOMETRIC_PRESENTATION_REPRESENTATION (  '', ( #3477 ), #1358 ) ;
#1012 = AXIS2_PLACEMENT_3D ( 'NONE', #3436, #4689, #4988 ) ;
#1013 = DIRECTION ( 'NONE',  ( 5.551115123125772841E-17, -1.848892746611743135E-31, -1.000000000000000000 ) ) ;
#1014 = CARTESIAN_POINT ( 'NONE',  ( -36.58361131987991399, 0.000000000000000000, 532.6725316595221784 ) ) ;
#1015 = CARTESIAN_POINT ( 'NONE',  ( 0.000000000000000000, 80.00000000000000000, -50.00000000000000000 ) ) ;
#1016 = DIRECTION ( 'NONE',  ( 0.000000000000000000, -1.000000000000000000, -0.000000000000000000 ) ) ;
#1017 = CARTESIAN_POINT ( 'NONE',  ( 5.624351423727524946, 2.222614453595284090E-15, 474.0483466084679662 ) ) ;
#1018 = ORIENTED_EDGE ( 'NONE', *, *, #1653, .F. ) ;
#1019 = CARTESIAN_POINT ( 'NONE',  ( 23.50217280487988347, 25.00000000000018474, 428.9062724124379997 ) ) ;
#1020 = ORIENTED_EDGE ( 'NONE', *, *, #1917, .F. ) ;
#1021 = CARTESIAN_POINT ( 'NONE',  ( -38.26122282208105219, 0.000000000000000000, 67.09613410133258071 ) ) ;
#1022 = VECTOR ( 'NONE', #4134, 1000.000000000000114 ) ;
#1023 = DIRECTION ( 'NONE',  ( -1.000000000000000000, 2.523234146875361914E-16, -5.551115123125772841E-17 ) ) ;
#1024 = ORIENTED_EDGE ( 'NONE', *, *, #4393, .F. ) ;
#1025 = EDGE_LOOP ( 'NONE', ( #3853, #1190, #2161 ) ) ;
#1026 = CARTESIAN_POINT ( 'NONE',  ( 0.000000000000000000, 80.00000000000000000, 0.000000000000000000 ) ) ;
#1027 = CARTESIAN_POINT ( 'NONE',  ( -351.5485029915759583, 2.222614453595284090E-15, 177.1955551554592603 ) ) ;
#1028 = DIRECTION ( 'NONE',  ( 0.000000000000000000, 1.000000000000000000, 0.000000000000000000 ) ) ;
#1029 = CIRCLE ( 'NONE', #2961, 1.000000000000000888 ) ;
#1030 = EDGE_CURVE ( 'NONE', #1903, #5244, #3739, .T. ) ;
#1031 = CARTESIAN_POINT ( 'NONE',  ( -315.9326898068451897, 4.999156891862612154E-15, 40.93645626314877717 ) ) ;
#1032 = ORIENTED_EDGE ( 'NONE', *, *, #4823, .F. ) ;
#1033 = EDGE_CURVE ( 'NONE', #3599, #3314, #4433, .T. ) ;
#1034 = EDGE_CURVE ( 'NONE', #3745, #744, #5128, .T. ) ;
#1035 = CARTESIAN_POINT ( 'NONE',  ( -376.1691690517220081, 2.222614453595299473E-15, 134.6976398800616437 ) ) ;
#1036 = EDGE_CURVE ( 'NONE', #4330, #921, #4093, .T. ) ;
#1037 = CARTESIAN_POINT ( 'NONE',  ( -334.2906958041451162, -25.00000000000003197, 430.9840019716597226 ) ) ;
#1038 = CARTESIAN_POINT ( 'NONE',  ( -338.5986743560152377, -14.95948628165117178, 39.80450035817695209 ) ) ;
#1039 = DIRECTION ( 'NONE',  ( -0.09383933793885568253, 2.673190762809473730E-31, 0.9955873536034882676 ) ) ;
#1040 = LINE ( 'NONE', #1062, #2701 ) ;
#1041 = CARTESIAN_POINT ( 'NONE',  ( 31.14585677005082687, 2.222614453595284090E-15, 398.7793066466531968 ) ) ;
#1042 = VERTEX_POINT ( 'NONE', #4491 ) ;
#1043 = CARTESIAN_POINT ( 'NONE',  ( -57.28677601057306390, 25.00000000000018474, 546.4981013186294376 ) ) ;
#1044 = ORIENTED_EDGE ( 'NONE', *, *, #796, .F. ) ;
#1045 = FACE_OUTER_BOUND ( 'NONE', #3554, .T. ) ;
#1046 = EDGE_CURVE ( 'NONE', #3719, #1423, #691, .T. ) ;
#1047 = EDGE_LOOP ( 'NONE', ( #5067, #3342 ) ) ;
#1048 = ORIENTED_EDGE ( 'NONE', *, *, #2914, .F. ) ;
#1049 = DIRECTION ( 'NONE',  ( -0.09383933793885537722, 2.626968444144180508E-31, 0.9955873536034883786 ) ) ;
#1050 = DIRECTION ( 'NONE',  ( 0.01527226085271977431, 2.087708059715749652E-31, 0.9998833722232041143 ) ) ;
#1051 = DIRECTION ( 'NONE',  ( 0.09383933793885537722, -2.626968444144180508E-31, -0.9955873536034883786 ) ) ;
#1052 = LINE ( 'NONE', #3948, #5201 ) ;
#1053 = FACE_OUTER_BOUND ( 'NONE', #2214, .T. ) ;
#1054 = ORIENTED_EDGE ( 'NONE', *, *, #399, .F. ) ;
#1055 = AXIS2_PLACEMENT_3D ( 'NONE', #1273, #3419, #2996 ) ;
#1056 = ADVANCED_FACE ( 'NONE', ( #1077 ), #5329, .T. ) ;
#1057 = CARTESIAN_POINT ( 'NONE',  ( 18.31346110193232590, 2.222614453595284090E-15, 444.2932575970293101 ) ) ;
#1058 = FACE_OUTER_BOUND ( 'NONE', #794, .T. ) ;
#1059 = CYLINDRICAL_SURFACE ( 'NONE', #3018, 14.00000000000002665 ) ;
#1060 = EDGE_CURVE ( 'NONE', #339, #1068, #4635, .T. ) ;
#1061 = AXIS2_PLACEMENT_3D ( 'NONE', #3273, #5260, #267 ) ;
#1062 = CARTESIAN_POINT ( 'NONE',  ( 102.9433289385998478, 0.000000000000000000, 135.9081080810072137 ) ) ;
#1063 = CARTESIAN_POINT ( 'NONE',  ( -367.0882437885061904, 2.222614453595284090E-15, 297.8351940652699454 ) ) ;
#1064 = SHAPE_DEFINITION_REPRESENTATION ( #5391, #2334 ) ;
#1065 = CARTESIAN_POINT ( 'NONE',  ( -23.53079058812344471, -24.99999999999981881, 476.4235034963351154 ) ) ;
#1066 = VERTEX_POINT ( 'NONE', #4004 ) ;
#1067 = CARTESIAN_POINT ( 'NONE',  ( -5.157059352427092236, 25.00000000000018474, 435.5986320196304860 ) ) ;
#1068 = VERTEX_POINT ( 'NONE', #2376 ) ;
#1069 = CIRCLE ( 'NONE', #3360, 31.50000000000120082 ) ;
#1070 = CARTESIAN_POINT ( 'NONE',  ( -81.77293133282597637, 75.50260479418152215, -10.00000000000000888 ) ) ;
#1071 = VECTOR ( 'NONE', #4116, 1000.000000000000000 ) ;
#1072 = VERTEX_POINT ( 'NONE', #750 ) ;
#1073 = VECTOR ( 'NONE', #5027, 1000.000000000000000 ) ;
#1074 = VECTOR ( 'NONE', #2811, 1000.000000000000000 ) ;
#1075 = ORIENTED_EDGE ( 'NONE', *, *, #3017, .F. ) ;
#1076 = CARTESIAN_POINT ( 'NONE',  ( -80.02857808274401918, 80.45434506795689344, -2.000000000000112799 ) ) ;
#1077 = FACE_OUTER_BOUND ( 'NONE', #5137, .T. ) ;
#1078 = DIRECTION ( 'NONE',  ( -5.551115123125772841E-17, 1.848892746611743135E-31, 1.000000000000000000 ) ) ;
#1079 = CARTESIAN_POINT ( 'NONE',  ( -338.5986743560152377, 2.276824562219559311E-15, 39.80450035817695209 ) ) ;
#1080 = MECHANICAL_DESIGN_GEOMETRIC_PRESENTATION_REPRESENTATION (  '', ( #2751 ), #1786 ) ;
#1081 = CARTESIAN_POINT ( 'NONE',  ( -332.4241159867397073, 5.421010862426837463E-17, 198.0823409706411553 ) ) ;
#1082 = ORIENTED_EDGE ( 'NONE', *, *, #1325, .T. ) ;
#1083 = EDGE_CURVE ( 'NONE', #4995, #4404, #1489, .T. ) ;
#1084 = DIRECTION ( 'NONE',  ( 0.000000000000000000, -1.000000000000000000, 0.000000000000000000 ) ) ;
#1085=STYLED_ITEM('',(#5451),#4927);
#1086 = CARTESIAN_POINT ( 'NONE',  ( -78.28422483266231779, -26.49739520581859153, -10.00000000000006395 ) ) ;
#1087 = CIRCLE ( 'NONE', #4172, 6.000000000000032863 ) ;
#1088 = DIRECTION ( 'NONE',  ( 0.000000000000000000, 0.000000000000000000, 1.000000000000000000 ) ) ;
#1089 = CARTESIAN_POINT ( 'NONE',  ( -353.3314504124138011, 0.000000000000000000, 196.1117148739250808 ) ) ;
#1090 = TOROIDAL_SURFACE ( 'NONE', #4175, 30.50000000000110845, 1.000000000000000000 ) ;
#1091 = CARTESIAN_POINT ( 'NONE',  ( 136.6230329513293213, 75.92317977368846016, -10.00000000000006395 ) ) ;
#1092 = AXIS2_PLACEMENT_3D ( 'NONE', #3410, #5065, #1307 ) ;
#1093 = DIRECTION ( 'NONE',  ( -0.9955873536034883786, 5.499036814894887477E-31, -0.09383933793885500252 ) ) ;
#1094 = CARTESIAN_POINT ( 'NONE',  ( 12.58979647763662513, 25.00000000000000355, 97.46177917735926144 ) ) ;
#1095 = DIRECTION ( 'NONE',  ( 0.3430150920801929293, 0.000000000000000000, 0.9393298923196348182 ) ) ;
#1096 = CARTESIAN_POINT ( 'NONE',  ( 23.50217280487988347, -24.99999999999981881, 428.9062724124379997 ) ) ;
#1097 = LINE ( 'NONE', #3451, #3193 ) ;
#1098 = ORIENTED_EDGE ( 'NONE', *, *, #244, .F. ) ;
#1099 = CARTESIAN_POINT ( 'NONE',  ( -330.1866567701607096, 24.99999999999997158, 374.2973685668110306 ) ) ;
#1100 = ORIENTED_EDGE ( 'NONE', *, *, #1377, .T. ) ;
#1101 = ADVANCED_FACE ( 'NONE', ( #2844, #4838 ), #286, .T. ) ;
#1102 = ADVANCED_FACE ( 'NONE', ( #1468, #1552 ), #233, .F. ) ;
#1103 = DIRECTION ( 'NONE',  ( 0.000000000000000000, 1.000000000000000000, 0.000000000000000000 ) ) ;
#1104 = DIRECTION ( 'NONE',  ( 5.551115123125772841E-17, -1.848892746611743135E-31, -1.000000000000000000 ) ) ;
#1105 = EDGE_LOOP ( 'NONE', ( #22, #441 ) ) ;
#1106 = EDGE_LOOP ( 'NONE', ( #2899, #3300, #4791, #1762 ) ) ;
#1107 = CARTESIAN_POINT ( 'NONE',  ( -17.84624325233685127, 4.358724120770097062E-15, 36.40401889739442254 ) ) ;
#1108 = DIRECTION ( 'NONE',  ( 0.09383933793885568253, -2.673190762809473730E-31, -0.9955873536034882676 ) ) ;
#1109 = DIRECTION ( 'NONE',  ( 0.09383933793885537722, -2.626968444144180508E-31, -0.9955873536034883786 ) ) ;
#1110 = CARTESIAN_POINT ( 'NONE',  ( 133.9714219172562366, -21.54565493204319182, -12.00000000000006573 ) ) ;
#1111 = PRODUCT_RELATED_PRODUCT_CATEGORY ( 'part', '', ( #787 ) ) ;
#1112 = DIRECTION ( 'NONE',  ( -5.551115123125772841E-17, 1.848892746611743135E-31, 1.000000000000000000 ) ) ;
#1113 = ORIENTED_EDGE ( 'NONE', *, *, #1498, .T. ) ;
#1114 = CIRCLE ( 'NONE', #4194, 17.00000000000009948 ) ;
#1115 = CARTESIAN_POINT ( 'NONE',  ( 29.23877717791895492, -14.99999999999998579, 67.09613410133256650 ) ) ;
#1116 = DIRECTION ( 'NONE',  ( 0.4205749795070160002, -0.9072577839912275843, -5.551115123125780237E-17 ) ) ;
#1117 = CARTESIAN_POINT ( 'NONE',  ( -77.50517668553013095, -14.99999999999998579, 131.6034880481681171 ) ) ;
#1118 = CARTESIAN_POINT ( 'NONE',  ( 131.3198108831832371, 84.98551036222518462, -11.99999999999995559 ) ) ;
#1119 = CARTESIAN_POINT ( 'NONE',  ( -13.17877320795252238, 3.807633061153782584E-15, 47.33401081801162746 ) ) ;
#1120 = AXIS2_PLACEMENT_3D ( 'NONE', #4477, #4908, #1093 ) ;
#1121 = FACE_OUTER_BOUND ( 'NONE', #5169, .T. ) ;
#1122 = CARTESIAN_POINT ( 'NONE',  ( -268.5984117390373171, 24.99999999999997158, 475.6392848759601293 ) ) ;
#1123 = CARTESIAN_POINT ( 'NONE',  ( -367.0460729392618191, -24.99999999999981881, 268.0688838304706678 ) ) ;
#1124 = CARTESIAN_POINT ( 'NONE',  ( -342.9618789639491752, -14.95948628165117178, 39.39324540378412109 ) ) ;
#1125 = CIRCLE ( 'NONE', #4204, 4.382543221487789964 ) ;
#1126 = VERTEX_POINT ( 'NONE', #4522 ) ;
#1127 = CARTESIAN_POINT ( 'NONE',  ( -342.0170653153610374, 25.00000000000018474, 268.9367132353194734 ) ) ;
#1128 = EDGE_LOOP ( 'NONE', ( #79, #4658, #3456, #2909 ) ) ;
#1129 = ADVANCED_FACE ( 'NONE', ( #4920 ), #4814, .T. ) ;
#1130 = LINE ( 'NONE', #3260, #913 ) ;
#1131 = ADVANCED_FACE ( 'NONE', ( #638, #2318, #1905, #2758, #1219 ), #444, .T. ) ;
#1132 = EDGE_CURVE ( 'NONE', #2756, #3474, #4626, .T. ) ;
#1133 = ORIENTED_EDGE ( 'NONE', *, *, #1696, .T. ) ;
#1134 = ADVANCED_FACE ( 'NONE', ( #1629 ), #3319, .F. ) ;
#1135 = ORIENTED_EDGE ( 'NONE', *, *, #826, .F. ) ;
#1136 = PRODUCT ( 'Base Mounting Flange Control Box Bracket small', 'Base Mounting Flange Control Box Bracket small', '', ( #1920 ) ) ;
#1137 = CARTESIAN_POINT ( 'NONE',  ( -66.30461487616335603, 15.00000000000001421, 161.8139267001887447 ) ) ;
#1138 = DIRECTION ( 'NONE',  ( 0.000000000000000000, 1.000000000000000000, 0.000000000000000000 ) ) ;
#1139 = CARTESIAN_POINT ( 'NONE',  ( -329.5232379498077080, 5.421010862427522170E-17, 102.9347045701690604 ) ) ;
#1140 = DIRECTION ( 'NONE',  ( 5.551115123125772841E-17, -1.848892746611743135E-31, -1.000000000000000000 ) ) ;
#1141 = DIRECTION ( 'NONE',  ( 0.09383933793885568253, -2.673190762809473730E-31, -0.9955873536034882676 ) ) ;
#1142 = VERTEX_POINT ( 'NONE', #420 ) ;
#1143 = FILL_AREA_STYLE_COLOUR ( '', #2947 ) ;
#1144 = LINE ( 'NONE', #2853, #3382 ) ;
#1145 = CARTESIAN_POINT ( 'NONE',  ( 0.000000000000000000, 0.000000000000000000, 0.000000000000000000 ) ) ;
#1146 = CARTESIAN_POINT ( 'NONE',  ( -365.9639710083354203, 1.530808498934204340E-15, 196.9298978568966163 ) ) ;
#1147 = SURFACE_STYLE_USAGE ( .BOTH. , #14 ) ;
#1148 = CARTESIAN_POINT ( 'NONE',  ( -376.2299595452952303, 1.264661897981941762E-29, 193.9534101013312863 ) ) ;
#1149 = CARTESIAN_POINT ( 'NONE',  ( -39.32426838450110296, 25.00000000000018474, 499.4571537926176461 ) ) ;
#1150 = CARTESIAN_POINT ( 'NONE',  ( -57.28677601057280100, 3.252606517456513302E-16, 546.4981013186296650 ) ) ;
#1151 = VERTEX_POINT ( 'NONE', #4140 ) ;
#1152 = CARTESIAN_POINT ( 'NONE',  ( -13.17877320795229856, 25.00000000000000355, 47.33401081801169141 ) ) ;
#1153 = ORIENTED_EDGE ( 'NONE', *, *, #5271, .T. ) ;
#1154 = DIRECTION ( 'NONE',  ( -1.000000000000000000, 0.000000000000000000, -5.551115123125777155E-17 ) ) ;
#1155 = FILL_AREA_STYLE ('',( #3146 ) ) ;
#1156 = EDGE_CURVE ( 'NONE', #2554, #1574, #4891, .T. ) ;
#1157 = AXIS2_PLACEMENT_3D ( 'NONE', #2494, #428, #3777 ) ;
#1158 = ORIENTED_EDGE ( 'NONE', *, *, #2207, .T. ) ;
#1159 = UNCERTAINTY_MEASURE_WITH_UNIT (LENGTH_MEASURE( 1.000000000000000082E-05 ), #1725, 'distance_accuracy_value', 'NONE');
#1160 = VERTEX_POINT ( 'NONE', #4550 ) ;
#1161 = AXIS2_PLACEMENT_3D ( 'NONE', #3304, #2768, #1943 ) ;
#1162 = CYLINDRICAL_SURFACE ( 'NONE', #2574, 27.50000000000126477 ) ;
#1163 = AXIS2_PLACEMENT_3D ( 'NONE', #838, #4576, #3345 ) ;
#1164 = DIRECTION ( 'NONE',  ( -0.9955873536034882676, 5.475514420260265162E-31, -0.09383933793885552987 ) ) ;
#1165 = FACE_OUTER_BOUND ( 'NONE', #5126, .T. ) ;
#1166 = FACE_OUTER_BOUND ( 'NONE', #2458, .T. ) ;
#1167 = CARTESIAN_POINT ( 'NONE',  ( -344.4167133082243595, 2.222614453595284090E-15, 101.5309162815936048 ) ) ;
#1168 = EDGE_LOOP ( 'NONE', ( #4715, #748, #3966, #4890 ) ) ;
#1169 = AXIS2_PLACEMENT_3D ( 'NONE', #3003, #2596, #4711 ) ;
#1170 = CIRCLE ( 'NONE', #4070, 77.49999999999998579 ) ;
#1171 = FILL_AREA_STYLE_COLOUR ( '', #2941 ) ;
#1172 = FACE_OUTER_BOUND ( 'NONE', #4283, .T. ) ;
#1173 = FACE_OUTER_BOUND ( 'NONE', #767, .T. ) ;
#1174 = DIRECTION ( 'NONE',  ( 0.9955873536034882676, -5.502656983963330823E-31, 0.09383933793885547436 ) ) ;
#1175 = AXIS2_PLACEMENT_3D ( 'NONE', #34, #446, #3755 ) ;
#1176 = VECTOR ( 'NONE', #2186, 1000.000000000000000 ) ;
#1177 = VECTOR ( 'NONE', #1492, 1000.000000000000000 ) ;
#1178 = DIRECTION ( 'NONE',  ( 5.551115123125772841E-17, -1.848892746611743354E-31, -1.000000000000000000 ) ) ;
#1179 = CARTESIAN_POINT ( 'NONE',  ( -68.63039925413373510, 25.00000000000018474, 524.1455590405155363 ) ) ;
#1180 = CARTESIAN_POINT ( 'NONE',  ( -223.9642223310785312, 5.421010862427522170E-17, 534.3227077389987016 ) ) ;
#1181 = AXIS2_PLACEMENT_3D ( 'NONE', #2660, #2713, #2225 ) ;
#1182 = PRODUCT_RELATED_PRODUCT_CATEGORY ( 'part', '', ( #3007 ) ) ;
#1183 = AXIS2_PLACEMENT_3D ( 'NONE', #925, #4279, #511 ) ;
#1184 = ORIENTED_EDGE ( 'NONE', *, *, #5158, .F. ) ;
#1185 = CARTESIAN_POINT ( 'NONE',  ( -364.1439395362590403, 25.00000000000018474, 237.2787335496889227 ) ) ;
#1186 = ORIENTED_EDGE ( 'NONE', *, *, #159, .F. ) ;
#1187 = AXIS2_PLACEMENT_3D ( 'NONE', #4006, #321, #4923 ) ;
#1188 = DIRECTION ( 'NONE',  ( 0.09383933793885568253, -2.673190762809473730E-31, -0.9955873536034882676 ) ) ;
#1189 = DIRECTION ( 'NONE',  ( -0.9955873536034882676, 5.498529991225543472E-31, -0.09383933793885566865 ) ) ;
#1190 = ORIENTED_EDGE ( 'NONE', *, *, #4135, .T. ) ;
#1191 = ORIENTED_EDGE ( 'NONE', *, *, #2031, .F. ) ;
#1192 = DIRECTION ( 'NONE',  ( 4.476705744456277327E-17, 0.000000000000000000, 1.000000000000000000 ) ) ;
#1193 = DIRECTION ( 'NONE',  ( -0.09383933793885568253, 2.673190762809473730E-31, 0.9955873536034882676 ) ) ;
#1194 = CARTESIAN_POINT ( 'NONE',  ( -86.02857808274421814, -21.54565493204321669, -2.000000000000002220 ) ) ;
#1195 = DIRECTION ( 'NONE',  ( 1.000000000000000000, -5.720779902258384700E-31, 0.000000000000000000 ) ) ;
#1196 = CARTESIAN_POINT ( 'NONE',  ( 137.9714219172561229, -39.54565493204319182, 152.0000000000004263 ) ) ;
#1197 = ORIENTED_EDGE ( 'NONE', *, *, #4921, .T. ) ;
#1198 = EDGE_CURVE ( 'NONE', #1846, #1622, #3771, .T. ) ;
#1199 = VERTEX_POINT ( 'NONE', #2120 ) ;
#1200 = CARTESIAN_POINT ( 'NONE',  ( -77.37696704867111919, -26.07682022631158247, -11.99999999999995559 ) ) ;
#1201 = CARTESIAN_POINT ( 'NONE',  ( -264.1404626571534777, 2.222614453595284090E-15, 511.7445549721628595 ) ) ;
#1202 = DIRECTION ( 'NONE',  ( 0.09383933793885537722, -2.626968444144180508E-31, -0.9955873536034883786 ) ) ;
#1203 = EDGE_CURVE ( 'NONE', #860, #342, #854, .T. ) ;
#1204 = ADVANCED_FACE ( 'NONE', ( #1240 ), #2364, .F. ) ;
#1205 = CARTESIAN_POINT ( 'NONE',  ( 127.9714219172562508, 80.45434506795683660, -2.000000000000002220 ) ) ;
#1206 = EDGE_CURVE ( 'NONE', #278, #3702, #4220, .T. ) ;
#1207 = EDGE_CURVE ( 'NONE', #2477, #3339, #1845, .T. ) ;
#1208 = FACE_OUTER_BOUND ( 'NONE', #5242, .T. ) ;
#1209 = CARTESIAN_POINT ( 'NONE',  ( -342.0244061588616091, 25.00000000000018474, 297.0039604601892620 ) ) ;
#1210 = CARTESIAN_POINT ( 'NONE',  ( 31.14585677005082687, 2.222614453595284090E-15, 398.7793066466531968 ) ) ;
#1211 = EDGE_CURVE ( 'NONE', #2228, #4995, #4980, .T. ) ;
#1212 = EDGE_LOOP ( 'NONE', ( #3502, #3142, #3219, #4157 ) ) ;
#1213 = EDGE_LOOP ( 'NONE', ( #880, #2719 ) ) ;
#1214 = CLOSED_SHELL ( 'NONE', ( #161, #183, #3754, #4160, #1928, #3466, #1769, #485, #563, #3808, #4728, #897, #1056, #1204, #2012, #3566, #1372, #4597, #4487, #3912, #3176, #3259, #5092, #4389, #2360, #4563, #3138, #1871, #5086, #60, #1765, #5253, #623, #1624, #558, #2030, #403, #4029, #5361, #675, #4962, #255, #1764, #1456, #1939, #1540, #3155, #5141, #879, #4061, #862, #2601, #540, #4760, #2106, #2608, #3346, #4967, #2180, #1129 ) ) ;
#1215 = FACE_OUTER_BOUND ( 'NONE', #5269, .T. ) ;
#1216 = DIRECTION ( 'NONE',  ( -0.9955873536034883786, 5.498529991225534714E-31, -0.09383933793885515517 ) ) ;
#1217 = EDGE_LOOP ( 'NONE', ( #1394, #3494, #4687, #1342 ) ) ;
#1218 = CARTESIAN_POINT ( 'NONE',  ( -80.02857808274401918, 80.45434506795689344, -2.000000000000112799 ) ) ;
#1219 = FACE_OUTER_BOUND ( 'NONE', #3407, .T. ) ;
#1220 = DIRECTION ( 'NONE',  ( 0.000000000000000000, -1.000000000000000000, 0.000000000000000000 ) ) ;
#1221 = EDGE_CURVE ( 'NONE', #4306, #742, #4913, .T. ) ;
#1222 = DIRECTION ( 'NONE',  ( 0.4205749795070160002, -0.9072577839912275843, -5.551115123125780237E-17 ) ) ;
#1223 = ORIENTED_EDGE ( 'NONE', *, *, #4128, .T. ) ;
#1224 = ORIENTED_EDGE ( 'NONE', *, *, #4717, .F. ) ;
#1225 = CARTESIAN_POINT ( 'NONE',  ( -322.0642881118418472, 5.421010862426285877E-17, 200.0632413726019649 ) ) ;
#1226 = FACE_OUTER_BOUND ( 'NONE', #188, .T. ) ;
#1227 = DIRECTION ( 'NONE',  ( 0.000000000000000000, 1.000000000000000000, 0.000000000000000000 ) ) ;
#1228 = EDGE_CURVE ( 'NONE', #2722, #1390, #431, .T. ) ;
#1229 = CARTESIAN_POINT ( 'NONE',  ( 16.14979140325228357, 2.276824562219547873E-15, 35.88476202840195839 ) ) ;
#1230 = EDGE_CURVE ( 'NONE', #463, #3842, #2802, .T. ) ;
#1231 = CARTESIAN_POINT ( 'NONE',  ( 0.07030049710132768581, 1.843143693225357538E-15, 219.5055207296747710 ) ) ;
#1232 = CARTESIAN_POINT ( 'NONE',  ( -299.8611223228771792, -25.00000000000003197, 439.6443911606498887 ) ) ;
#1233 = CARTESIAN_POINT ( 'NONE',  ( 133.9714219172562650, 80.45434506795682239, -9.999999999999841904 ) ) ;
#1234 = ORIENTED_EDGE ( 'NONE', *, *, #2105, .F. ) ;
#1235 = LINE ( 'NONE', #3258, #3798 ) ;
#1236 = CARTESIAN_POINT ( 'NONE',  ( -323.7051989975983588, 2.222614453595284090E-15, 41.20828864675230108 ) ) ;
#1237 = ORIENTED_EDGE ( 'NONE', *, *, #3823, .T. ) ;
#1238 = ORIENTED_EDGE ( 'NONE', *, *, #3499, .T. ) ;
#1239 = LINE ( 'NONE', #5028, #3287 ) ;
#1240 = FACE_OUTER_BOUND ( 'NONE', #1378, .T. ) ;
#1241 = FACE_OUTER_BOUND ( 'NONE', #3846, .T. ) ;
#1242 = DIRECTION ( 'NONE',  ( 5.551115123125772841E-17, -1.848892746611743135E-31, -1.000000000000000000 ) ) ;
#1243 = AXIS2_PLACEMENT_3D ( 'NONE', #4099, #4531, #2469 ) ;
#1244 = ORIENTED_EDGE ( 'NONE', *, *, #2013, .F. ) ;
#1245 = AXIS2_PLACEMENT_3D ( 'NONE', #3918, #3091, #1950 ) ;
#1246 = ORIENTED_EDGE ( 'NONE', *, *, #1854, .F. ) ;
#1247 = CARTESIAN_POINT ( 'NONE',  ( -319.3063019478910292, 4.060433389145217710E-15, 160.1459078905241427 ) ) ;
#1248 = CARTESIAN_POINT ( 'NONE',  ( 151.9714219172563219, 84.45434506795677976, -5.551115123125782702E-14 ) ) ;
#1249 = AXIS2_PLACEMENT_3D ( 'NONE', #4787, #1103, #225 ) ;
#1250 = ADVANCED_FACE ( 'NONE', ( #4168 ), #4575, .F. ) ;
#1251 = CARTESIAN_POINT ( 'NONE',  ( -63.04765821499436385, 1.843143693225357538E-15, 521.0401840782876661 ) ) ;
#1252 = AXIS2_PLACEMENT_3D ( 'NONE', #4037, #5290, #4418 ) ;
#1253 = CARTESIAN_POINT ( 'NONE',  ( -330.1866567701584927, 3.740497495074990297E-15, 374.2973685668102917 ) ) ;
#1254 = VECTOR ( 'NONE', #3150, 1000.000000000000000 ) ;
#1255 = CARTESIAN_POINT ( 'NONE',  ( -5.157059352426552223, 3.740497495074990297E-15, 435.5986320196309975 ) ) ;
#1256 = CARTESIAN_POINT ( 'NONE',  ( -367.0882437885061904, 2.222614453595284090E-15, 297.8351940652699454 ) ) ;
#1257 = AXIS2_PLACEMENT_3D ( 'NONE', #3286, #5022, #4211 ) ;
#1258 = MECHANICAL_DESIGN_GEOMETRIC_PRESENTATION_REPRESENTATION (  '', ( #1613 ), #4081 ) ;
#1259 = ORIENTED_EDGE ( 'NONE', *, *, #2015, .F. ) ;
#1260 = CARTESIAN_POINT ( 'NONE',  ( 128.7214219172562650, 80.45434506795679397, -2.000000000000002220 ) ) ;
#1261 = CIRCLE ( 'NONE', #1695, 23.00000000000121503 ) ;
#1262 = AXIS2_PLACEMENT_3D ( 'NONE', #1606, #2117, #27 ) ;
#1263 = DIRECTION ( 'NONE',  ( 0.09383933793885568253, -2.673190762809473730E-31, -0.9955873536034882676 ) ) ;
#1264 = EDGE_CURVE ( 'NONE', #1807, #697, #3307, .T. ) ;
#1265 = ORIENTED_EDGE ( 'NONE', *, *, #3424, .T. ) ;
#1266 = EDGE_CURVE ( 'NONE', #4306, #861, #2859, .T. ) ;
#1267 = AXIS2_PLACEMENT_3D ( 'NONE', #5287, #4066, #327 ) ;
#1268 = PLANE ( 'NONE',  #1958 ) ;
#1269 = CARTESIAN_POINT ( 'NONE',  ( 132.2270686671743647, -26.49739520581860219, -9.999999999999953815 ) ) ;
#1270 = DIRECTION ( 'NONE',  ( -0.9955873536034883786, 5.498529991225534714E-31, -0.09383933793885515517 ) ) ;
#1271 = DIRECTION ( 'NONE',  ( -1.000000000000000000, 0.000000000000000000, 0.000000000000000000 ) ) ;
#1272 = PLANE ( 'NONE',  #3800 ) ;
#1273 = CARTESIAN_POINT ( 'NONE',  ( 29.23877717791899755, 15.00000000000001421, 67.09613410133263756 ) ) ;
#1274 = ORIENTED_EDGE ( 'NONE', *, *, #56, .F. ) ;
#1275 = ORIENTED_EDGE ( 'NONE', *, *, #129, .F. ) ;
#1276 = ORIENTED_EDGE ( 'NONE', *, *, #4199, .F. ) ;
#1277 = DIRECTION ( 'NONE',  ( 5.551115123125772841E-17, -1.848892746611743135E-31, -1.000000000000000000 ) ) ;
#1278 = DIRECTION ( 'NONE',  ( -5.551115123125772841E-17, 1.848892746611743135E-31, 1.000000000000000000 ) ) ;
#1279 = FACE_OUTER_BOUND ( 'NONE', #3860, .T. ) ;
#1280 = CARTESIAN_POINT ( 'NONE',  ( -351.6423423295148041, 5.421010862427522170E-17, 178.1911425090623311 ) ) ;
#1281 = FACE_OUTER_BOUND ( 'NONE', #2842, .T. ) ;
#1282 = CARTESIAN_POINT ( 'NONE',  ( -121.8424039465433566, -24.99999999999981881, 535.4314447305355316 ) ) ;
#1283 = FACE_OUTER_BOUND ( 'NONE', #4595, .T. ) ;
#1284 = EDGE_CURVE ( 'NONE', #921, #4034, #2951, .T. ) ;
#1285 = MANIFOLD_SOLID_BREP ( 'Boss-Extrude9', #1214 ) ;
#1286 = EDGE_LOOP ( 'NONE', ( #2520, #4786, #1113, #206 ) ) ;
#1287 = EDGE_LOOP ( 'NONE', ( #51, #5185, #215, #4387 ) ) ;
#1288 = CARTESIAN_POINT ( 'NONE',  ( -349.7655555707375470, 2.222614453595284090E-15, 158.2793954369922176 ) ) ;
#1289 =( LENGTH_UNIT ( ) NAMED_UNIT ( * ) SI_UNIT ( .MILLI., .METRE. ) );
#1290 = VECTOR ( 'NONE', #4285, 1000.000000000000000 ) ;
#1291 = CARTESIAN_POINT ( 'NONE',  ( -98.02857808274411866, 84.45434506795672291, -12.00000000000001066 ) ) ;
#1292 = ORIENTED_EDGE ( 'NONE', *, *, #5426, .T. ) ;
#1293 = DIRECTION ( 'NONE',  ( -5.551115123125772841E-17, 1.848892746611743135E-31, 1.000000000000000000 ) ) ;
#1294 = AXIS2_PLACEMENT_3D ( 'NONE', #4874, #1108, #3676 ) ;
#1295 = ADVANCED_FACE ( 'NONE', ( #4529 ), #885, .F. ) ;
#1296 = DIRECTION ( 'NONE',  ( -0.9955873536034882676, 5.452307672560245432E-31, -0.09383933793885568253 ) ) ;
#1297 = DIRECTION ( 'NONE',  ( -0.4205749795070160557, 0.9072577839912276954, 5.551115123125780853E-17 ) ) ;
#1298 = FACE_OUTER_BOUND ( 'NONE', #259, .T. ) ;
#1299 = CARTESIAN_POINT ( 'NONE',  ( -383.7907040352601484, 1.677051647323856397E-29, 194.2452024203927294 ) ) ;
#1300 = ADVANCED_FACE ( 'NONE', ( #645 ), #4009, .T. ) ;
#1301 = EDGE_CURVE ( 'NONE', #2111, #1369, #1525, .T. ) ;
#1302 = ORIENTED_EDGE ( 'NONE', *, *, #1264, .F. ) ;
#1303 = ORIENTED_EDGE ( 'NONE', *, *, #2452, .F. ) ;
#1304 = EDGE_LOOP ( 'NONE', ( #2967, #2069, #343, #472 ) ) ;
#1305 = DIRECTION ( 'NONE',  ( -0.9955873536034882676, 5.498529991225532962E-31, -0.09383933793885514130 ) ) ;
#1306 = CARTESIAN_POINT ( 'NONE',  ( -353.3314504124138011, 0.000000000000000000, 196.1117148739250808 ) ) ;
#1307 = DIRECTION ( 'NONE',  ( -1.000000000000000000, 0.000000000000000000, 0.000000000000000000 ) ) ;
#1308 = MANIFOLD_SOLID_BREP ( 'Boss-Extrude1', #4374 ) ;
#1309 = FACE_OUTER_BOUND ( 'NONE', #47, .T. ) ;
#1310 = ORIENTED_EDGE ( 'NONE', *, *, #3718, .T. ) ;
#1311 = DIRECTION ( 'NONE',  ( 0.000000000000000000, 0.000000000000000000, 1.000000000000000000 ) ) ;
#1312 = CARTESIAN_POINT ( 'NONE',  ( 11.35554381053716000, 3.794707603699265519E-15, 353.5846600851142512 ) ) ;
#1313 = PLANE ( 'NONE',  #5033 ) ;
#1314 = ORIENTED_EDGE ( 'NONE', *, *, #4623, .F. ) ;
#1315 = ORIENTED_EDGE ( 'NONE', *, *, #823, .T. ) ;
#1316 = DIRECTION ( 'NONE',  ( 5.551115123125772841E-17, -1.848892746611743135E-31, -1.000000000000000000 ) ) ;
#1317 = AXIS2_PLACEMENT_3D ( 'NONE', #2589, #3849, #2639 ) ;
#1318 = DIRECTION ( 'NONE',  ( 5.551115123125772841E-17, -1.848892746611743135E-31, -1.000000000000000000 ) ) ;
#1319 = ORIENTED_EDGE ( 'NONE', *, *, #1746, .T. ) ;
#1320 = CARTESIAN_POINT ( 'NONE',  ( -382.1015959523611514, 5.421010862429199116E-17, 176.3246300555306050 ) ) ;
#1321 = DIRECTION ( 'NONE',  ( -0.9955873536034882676, 5.452307672560245432E-31, -0.09383933793885568253 ) ) ;
#1322 = CARTESIAN_POINT ( 'NONE',  ( -152.2642418387488874, -24.99999999999981881, 532.1805559224803801 ) ) ;
#1323 = SURFACE_SIDE_STYLE ('',( #2562 ) ) ;
#1324 = DIRECTION ( 'NONE',  ( -0.09383933793885536334, 2.611561004589082183E-31, 0.9955873536034882676 ) ) ;
#1325 = EDGE_CURVE ( 'NONE', #3769, #1738, #5399, .T. ) ;
#1326 = DIRECTION ( 'NONE',  ( 0.09383933793885568253, -2.673190762809473730E-31, -0.9955873536034882676 ) ) ;
#1327 = VERTEX_POINT ( 'NONE', #3187 ) ;
#1328 = EDGE_LOOP ( 'NONE', ( #3322, #1911, #2307, #683 ) ) ;
#1329 = ORIENTED_EDGE ( 'NONE', *, *, #4393, .T. ) ;
#1330 = CARTESIAN_POINT ( 'NONE',  ( -66.30461487616335603, 15.00000000000001421, 161.8139267001887447 ) ) ;
#1331 = DIRECTION ( 'NONE',  ( 1.000000000000000000, 0.000000000000000000, 0.000000000000000000 ) ) ;
#1332 = DIRECTION ( 'NONE',  ( -0.9955873536034882676, 5.498529991225538217E-31, -0.09383933793885536334 ) ) ;
#1333 = FACE_OUTER_BOUND ( 'NONE', #1168, .T. ) ;
#1334 = ORIENTED_EDGE ( 'NONE', *, *, #2457, .T. ) ;
#1335 = VECTOR ( 'NONE', #2052, 1000.000000000000000 ) ;
#1336 = EDGE_CURVE ( 'NONE', #2924, #3703, #1940, .T. ) ;
#1337 = DIRECTION ( 'NONE',  ( 0.000000000000000000, 0.000000000000000000, -1.000000000000000000 ) ) ;
#1338 = CARTESIAN_POINT ( 'NONE',  ( -249.5207023207451300, 1.843143693225357538E-15, 491.2832465756980014 ) ) ;
#1339 = DIRECTION ( 'NONE',  ( 0.09383933793885568253, -2.673190762809473730E-31, -0.9955873536034882676 ) ) ;
#1340 = CIRCLE ( 'NONE', #2127, 39.24395386344908587 ) ;
#1341 = MANIFOLD_SOLID_BREP ( 'Boss-Extrude1', #2530 ) ;
#1342 = ORIENTED_EDGE ( 'NONE', *, *, #2342, .F. ) ;
#1343 = VECTOR ( 'NONE', #112, 1000.000000000000000 ) ;
#1344 = AXIS2_PLACEMENT_3D ( 'NONE', #284, #4490, #4897 ) ;
#1345 = EDGE_LOOP ( 'NONE', ( #4290, #1184, #128, #5421 ) ) ;
#1346 = DIRECTION ( 'NONE',  ( 5.551115123125772841E-17, -1.848892746611743135E-31, -1.000000000000000000 ) ) ;
#1347 = DIRECTION ( 'NONE',  ( 1.000000000000000000, 0.000000000000000000, 0.000000000000000000 ) ) ;
#1348 = VECTOR ( 'NONE', #176, 1000.000000000000000 ) ;
#1349 = VERTEX_POINT ( 'NONE', #3245 ) ;
#1350 = CARTESIAN_POINT ( 'NONE',  ( 23.50217280488020677, 5.421010862427522170E-17, 428.9062724124374881 ) ) ;
#1351 = ORIENTED_EDGE ( 'NONE', *, *, #5184, .T. ) ;
#1352 = TOROIDAL_SURFACE ( 'NONE', #3898, 30.50000000000105516, 1.000000000000000000 ) ;
#1353 = VECTOR ( 'NONE', #2876, 1000.000000000000000 ) ;
#1354 = DIRECTION ( 'NONE',  ( -0.9955873536034883786, 5.498529991225532086E-31, -0.09383933793885522456 ) ) ;
#1355 = CARTESIAN_POINT ( 'NONE',  ( -107.0991749147294172, 1.572093150103981429E-15, 535.0680222229615310 ) ) ;
#1356 = CARTESIAN_POINT ( 'NONE',  ( -105.2090356704105147, 2.222614453595284090E-15, 560.1816718768288865 ) ) ;
#1357 = FACE_OUTER_BOUND ( 'NONE', #4733, .T. ) ;
#1358 =( GEOMETRIC_REPRESENTATION_CONTEXT ( 3 ) GLOBAL_UNCERTAINTY_ASSIGNED_CONTEXT ( ( #3647 ) ) GLOBAL_UNIT_ASSIGNED_CONTEXT ( ( #4930, #4844, #4062 ) ) REPRESENTATION_CONTEXT ( 'NONE', 'WORKASPACE' ) );
#1359 = AXIS2_PLACEMENT_3D ( 'NONE', #2253, #3471, #615 ) ;
#1360 = AXIS2_PLACEMENT_3D ( 'NONE', #1880, #4089, #1993 ) ;
#1361 = ORIENTED_EDGE ( 'NONE', *, *, #1034, .T. ) ;
#1362 = ORIENTED_EDGE ( 'NONE', *, *, #1228, .F. ) ;
#1363 = ORIENTED_EDGE ( 'NONE', *, *, #5123, .T. ) ;
#1364 = AXIS2_PLACEMENT_3D ( 'NONE', #3445, #5020, #437 ) ;
#1365 = DIRECTION ( 'NONE',  ( 0.9955873536034882676, 0.000000000000000000, 0.09383933793885600172 ) ) ;
#1366 = LINE ( 'NONE', #175, #4060 ) ;
#1367 = DIRECTION ( 'NONE',  ( 0.09383933793885536334, -2.626968444144180070E-31, -0.9955873536034882676 ) ) ;
#1368 = DIRECTION ( 'NONE',  ( 5.551115123125772841E-17, -1.848892746611743135E-31, -1.000000000000000000 ) ) ;
#1369 = VERTEX_POINT ( 'NONE', #4902 ) ;
#1370 = VECTOR ( 'NONE', #1084, 1000.000000000000000 ) ;
#1371 = LINE ( 'NONE', #3133, #2698 ) ;
#1372 = ADVANCED_FACE ( 'NONE', ( #3271 ), #1090, .T. ) ;
#1373 = CARTESIAN_POINT ( 'NONE',  ( 33.59898979596707136, -24.99999999999981881, 384.0431050523492900 ) ) ;
#1374 = DIRECTION ( 'NONE',  ( -0.9955873536034887117, 6.307420567868191288E-31, -0.09383933793885125552 ) ) ;
#1375 = ADVANCED_FACE ( 'NONE', ( #1987 ), #3715, .F. ) ;
#1376 = EDGE_CURVE ( 'NONE', #3842, #4320, #2913, .T. ) ;
#1377 = EDGE_CURVE ( 'NONE', #921, #964, #1571, .T. ) ;
#1378 = EDGE_LOOP ( 'NONE', ( #2611, #1754, #4716, #1054 ) ) ;
#1379 = DIRECTION ( 'NONE',  ( 1.000000000000000000, -3.759415251443877817E-31, 5.551115123125772841E-17 ) ) ;
#1380 = CARTESIAN_POINT ( 'NONE',  ( -338.5048350180761076, 2.276824562219559311E-15, 38.80891300457378890 ) ) ;
#1381 = ORIENTED_EDGE ( 'NONE', *, *, #1471, .T. ) ;
#1382 = CARTESIAN_POINT ( 'NONE',  ( -223.9642223310785312, 5.421010862427522170E-17, 534.3227077389987016 ) ) ;
#1383 = AXIS2_PLACEMENT_3D ( 'NONE', #1380, #2090, #1666 ) ;
#1384 = EDGE_LOOP ( 'NONE', ( #5327, #1507, #1441, #2191 ) ) ;
#1385 = DIRECTION ( 'NONE',  ( -1.000000000000000000, 0.000000000000000000, 0.000000000000000000 ) ) ;
#1386 = CARTESIAN_POINT ( 'NONE',  ( 12.58979647763662513, -25.00000000000000355, 97.46177917735926144 ) ) ;
#1387 = DIRECTION ( 'NONE',  ( 5.551115123125772841E-17, -1.848892746611743135E-31, -1.000000000000000000 ) ) ;
#1388 = CARTESIAN_POINT ( 'NONE',  ( 0.000000000000000000, 0.000000000000000000, 0.000000000000000000 ) ) ;
#1389 = CIRCLE ( 'NONE', #2086, 1.000000000000000888 ) ;
#1390 = VERTEX_POINT ( 'NONE', #3672 ) ;
#1391 = ORIENTED_EDGE ( 'NONE', *, *, #3564, .T. ) ;
#1392 = EDGE_CURVE ( 'NONE', #2971, #800, #4592, .T. ) ;
#1394 = ORIENTED_EDGE ( 'NONE', *, *, #320, .F. ) ;
#1393 = CIRCLE ( 'NONE', #2352, 14.00000000000002665 ) ;
#1395 = CARTESIAN_POINT ( 'NONE',  ( -344.4167133082243595, 2.222614453595284090E-15, 101.5309162815936048 ) ) ;
#1396 = CARTESIAN_POINT ( 'NONE',  ( 133.9714219172562366, 80.45434506795683660, -12.00000000000001066 ) ) ;
#1397 = DIRECTION ( 'NONE',  ( 5.551115123125772841E-17, -1.848892746611743135E-31, -1.000000000000000000 ) ) ;
#1398 = VERTEX_POINT ( 'NONE', #341 ) ;
#1399 = CARTESIAN_POINT ( 'NONE',  ( -36.58361131987999926, -24.99999999999981881, 532.6725316595209279 ) ) ;
#1400 = FACE_OUTER_BOUND ( 'NONE', #3859, .T. ) ;
#1401 = EDGE_CURVE ( 'NONE', #3100, #936, #2692, .T. ) ;
#1402 = AXIS2_PLACEMENT_3D ( 'NONE', #2873, #32, #3401 ) ;
#1403 = EDGE_CURVE ( 'NONE', #5281, #4568, #144, .T. ) ;
#1404 = CARTESIAN_POINT ( 'NONE',  ( -379.3436097884102765, 6.080251870909620328E-15, 136.4072965734520153 ) ) ;
#1405 = LINE ( 'NONE', #4318, #2081 ) ;
#1406 = ORIENTED_EDGE ( 'NONE', *, *, #1156, .T. ) ;
#1407 = CARTESIAN_POINT ( 'NONE',  ( -105.2090356704105147, 2.222614453595284090E-15, 560.1816718768288865 ) ) ;
#1408 = ORIENTED_EDGE ( 'NONE', *, *, #3721, .T. ) ;
#1409 = DIRECTION ( 'NONE',  ( 0.000000000000000000, 0.000000000000000000, 1.000000000000000000 ) ) ;
#1410 = CARTESIAN_POINT ( 'NONE',  ( -320.6447527397726276, 2.276824562219559311E-15, 453.8399743637901906 ) ) ;
#1411 = DIRECTION ( 'NONE',  ( 0.09383933793885568253, -2.673190762809473730E-31, -0.9955873536034882676 ) ) ;
#1412 = ORIENTED_EDGE ( 'NONE', *, *, #2648, .T. ) ;
#1413 = ORIENTED_EDGE ( 'NONE', *, *, #2066, .F. ) ;
#1414 = DIRECTION ( 'NONE',  ( -0.9983803615885644689, 0.000000000000000000, -0.05689159511111529371 ) ) ;
#1415 = DIRECTION ( 'NONE',  ( 0.000000000000000000, 0.000000000000000000, -1.000000000000000000 ) ) ;
#1416 = LINE ( 'NONE', #3218, #4854 ) ;
#1417 = EDGE_LOOP ( 'NONE', ( #584, #3489, #5139, #173 ) ) ;
#1418 = DIRECTION ( 'NONE',  ( 1.000000000000000000, -3.851859888774468203E-31, 0.000000000000000000 ) ) ;
#1419 = CARTESIAN_POINT ( 'NONE',  ( 23.50217280488020677, 5.421010862427522170E-17, 428.9062724124374881 ) ) ;
#1420 = CARTESIAN_POINT ( 'NONE',  ( 139.2214219172562366, 80.45434506795679397, -26.84924240491753977 ) ) ;
#1421 = CIRCLE ( 'NONE', #1504, 27.50000000000126121 ) ;
#1422 = CIRCLE ( 'NONE', #4589, 21.00000000000012790 ) ;
#1423 = VERTEX_POINT ( 'NONE', #3285 ) ;
#1424 = CARTESIAN_POINT ( 'NONE',  ( 5.624351423727398824, 25.00000000000018474, 474.0483466084681368 ) ) ;
#1425 = SHAPE_REPRESENTATION_RELATIONSHIP ( 'NONE' , 'NONE' ,  #2334, #2204 ) ;
#1426 = AXIS2_PLACEMENT_3D ( 'NONE', #1916, #5210, #1945 ) ;
#1427 = CIRCLE ( 'NONE', #3546, 4.382543221487789964 ) ;
#1428 = ORIENTED_EDGE ( 'NONE', *, *, #2582, .F. ) ;
#1429 = CARTESIAN_POINT ( 'NONE',  ( -36.58361131987999926, 25.00000000000018474, 532.6725316595209279 ) ) ;
#1430 = CIRCLE ( 'NONE', #4504, 21.00000000000124700 ) ;
#1431 = ORIENTED_EDGE ( 'NONE', *, *, #2648, .F. ) ;
#1432 = CARTESIAN_POINT ( 'NONE',  ( 29.23877717791896202, -14.99999999999998579, 17.09613410133256650 ) ) ;
#1433 = AXIS2_PLACEMENT_3D ( 'NONE', #3834, #4982, #3429 ) ;
#1434 = COLOUR_RGB ( '',0.7921568627450980005, 0.8196078431372548767, 0.9333333333333333481 ) ;
#1435 = EDGE_CURVE ( 'NONE', #195, #3013, #328, .T. ) ;
#1436 = EDGE_CURVE ( 'NONE', #4871, #3515, #5410, .T. ) ;
#1437 = AXIS2_PLACEMENT_3D ( 'NONE', #4217, #1023, #4327 ) ;
#1438 = VERTEX_POINT ( 'NONE', #4915 ) ;
#1439 = EDGE_CURVE ( 'NONE', #664, #3905, #3406, .T. ) ;
#1440 = AXIS2_PLACEMENT_3D ( 'NONE', #5013, #4184, #5044 ) ;
#1441 = ORIENTED_EDGE ( 'NONE', *, *, #4555, .T. ) ;
#1442 = FACE_BOUND ( 'NONE', #685, .T. ) ;
#1443 = DIRECTION ( 'NONE',  ( 0.9955873536034882676, 0.000000000000000000, 0.09383933793885600172 ) ) ;
#1444 = CARTESIAN_POINT ( 'NONE',  ( -38.26122282208105219, -14.99999999999998579, 67.09613410133258071 ) ) ;
#1445 = AXIS2_PLACEMENT_3D ( 'NONE', #469, #2150, #3421 ) ;
#1446 = TOROIDAL_SURFACE ( 'NONE', #1012, 28.50000000000115463, 1.000000000000000000 ) ;
#1447 = CIRCLE ( 'NONE', #214, 12.50000000000008704 ) ;
#1448 = CARTESIAN_POINT ( 'NONE',  ( -344.4167133082243595, -14.95948628165117178, 101.5309162815936048 ) ) ;
#1449 = VERTEX_POINT ( 'NONE', #4485 ) ;
#1450 = AXIS2_PLACEMENT_3D ( 'NONE', #2406, #4091, #2727 ) ;
#1451 = LINE ( 'NONE', #5129, #1290 ) ;
#1452 = CARTESIAN_POINT ( 'NONE',  ( -312.0566616799260373, -25.00000000000003197, 419.2731246273838792 ) ) ;
#1453 = DIRECTION ( 'NONE',  ( -1.000000000000000000, 0.000000000000000000, -7.228014483236656373E-17 ) ) ;
#1454 = CARTESIAN_POINT ( 'NONE',  ( -349.8593949086763928, 2.222614453595284090E-15, 159.2749827905956010 ) ) ;
#1455 = CARTESIAN_POINT ( 'NONE',  ( 133.9714219172562366, -21.54565493204319182, -2.000000000000001776 ) ) ;
#1456 = ADVANCED_FACE ( 'NONE', ( #4892 ), #1960, .T. ) ;
#1457 = CARTESIAN_POINT ( 'NONE',  ( 34.60640066538633874, 2.222614453595284090E-15, 295.6817845355787995 ) ) ;
#1458 = APPLICATION_PROTOCOL_DEFINITION ( 'draft international standard', 'automotive_design', 1998, #632 ) ;
#1459 = ORIENTED_EDGE ( 'NONE', *, *, #1534, .T. ) ;
#1460 = CARTESIAN_POINT ( 'NONE',  ( 29.77542608467492613, 2.222614453595284090E-15, 249.2409987768030533 ) ) ;
#1461 = ORIENTED_EDGE ( 'NONE', *, *, #5021, .T. ) ;
#1462 = CARTESIAN_POINT ( 'NONE',  ( 151.9714219172563219, 84.45434506795673713, 152.0000000000001990 ) ) ;
#1463 = DIRECTION ( 'NONE',  ( -0.9955873536034883786, 5.452307672560241053E-31, -0.09383933793885559926 ) ) ;
#1464 = ORIENTED_EDGE ( 'NONE', *, *, #460, .T. ) ;
#1465 = EDGE_CURVE ( 'NONE', #281, #742, #1235, .T. ) ;
#1466 = EDGE_LOOP ( 'NONE', ( #5338, #1334, #4557, #4632 ) ) ;
#1467 = CARTESIAN_POINT ( 'NONE',  ( 151.9714219172562935, -25.54565493204309234, -5.551115123125782702E-14 ) ) ;
#1468 = FACE_BOUND ( 'NONE', #337, .T. ) ;
#1469 = DIRECTION ( 'NONE',  ( -1.000000000000000000, 0.000000000000000000, 0.000000000000000000 ) ) ;
#1470 = CYLINDRICAL_SURFACE ( 'NONE', #910, 4.382543221487789964 ) ;
#1471 = EDGE_CURVE ( 'NONE', #4644, #689, #1430, .T. ) ;
#1472 = EDGE_LOOP ( 'NONE', ( #4622, #799 ) ) ;
#1473 = PRESENTATION_STYLE_ASSIGNMENT (( #3160 ) ) ;
#1474 = DIRECTION ( 'NONE',  ( -1.000000000000000000, 0.000000000000000000, -7.228014483236656373E-17 ) ) ;
#1475 = CARTESIAN_POINT ( 'NONE',  ( 36.66581985038887126, -24.99999999999981881, 340.1662229844756098 ) ) ;
#1476 = DIRECTION ( 'NONE',  ( 5.551115123125772841E-17, -1.848892746611743135E-31, -1.000000000000000000 ) ) ;
#1477 = PLANE ( 'NONE',  #2573 ) ;
#1478 = DIRECTION ( 'NONE',  ( -0.09383933793885568253, 2.673190762809473730E-31, 0.9955873536034882676 ) ) ;
#1479 = CARTESIAN_POINT ( 'NONE',  ( 23.50217280488020677, 5.421010862427522170E-17, 428.9062724124374881 ) ) ;
#1480 = CARTESIAN_POINT ( 'NONE',  ( -24.17433829723480443, -24.03864171390192439, 17.05778483357696373 ) ) ;
#1481 = CARTESIAN_POINT ( 'NONE',  ( -5.157059352427092236, -24.99999999999981881, 435.5986320196304860 ) ) ;
#1482 = ORIENTED_EDGE ( 'NONE', *, *, #2888, .F. ) ;
#1483 = CARTESIAN_POINT ( 'NONE',  ( -0.4023372602957597799, 1.572093150103981429E-15, 421.4664991284013809 ) ) ;
#1484 = ORIENTED_EDGE ( 'NONE', *, *, #3088, .F. ) ;
#1485 = DIRECTION ( 'NONE',  ( -1.000000000000000000, 0.000000000000000000, -5.551115123125782702E-17 ) ) ;
#1486 = VERTEX_POINT ( 'NONE', #2835 ) ;
#1487 = ORIENTED_EDGE ( 'NONE', *, *, #530, .T. ) ;
#1488 = CARTESIAN_POINT ( 'NONE',  ( 29.23877717791899400, 15.00000000000001421, -10.40386589866734646 ) ) ;
#1489 = LINE ( 'NONE', #200, #2003 ) ;
#1490 = DIRECTION ( 'NONE',  ( -0.4205749795070160002, 0.9072577839912275843, 5.551115123125780237E-17 ) ) ;
#1491 = CARTESIAN_POINT ( 'NONE',  ( 133.9714219172562650, 80.45434506795683660, -2.000000000000001776 ) ) ;
#1492 = DIRECTION ( 'NONE',  ( -5.551115123125772841E-17, 1.848892746611743135E-31, 1.000000000000000000 ) ) ;
#1493 = VERTEX_POINT ( 'NONE', #2509 ) ;
#1494 = LINE ( 'NONE', #4149, #372 ) ;
#1495 = FACE_OUTER_BOUND ( 'NONE', #4634, .T. ) ;
#1496 = ADVANCED_FACE ( 'NONE', ( #1215 ), #2428, .T. ) ;
#1497 = DIRECTION ( 'NONE',  ( 5.551115123125772841E-17, -1.848892746611743354E-31, -1.000000000000000000 ) ) ;
#1498 = EDGE_CURVE ( 'NONE', #2521, #3281, #466, .T. ) ;
#1499 = DIRECTION ( 'NONE',  ( -0.09383933793885568253, 2.673190762809473730E-31, 0.9955873536034882676 ) ) ;
#1500 = CARTESIAN_POINT ( 'NONE',  ( -320.6447527397726276, 2.276824562219559311E-15, 453.8399743637901906 ) ) ;
#1501 = SHAPE_DEFINITION_REPRESENTATION ( #2064, #4024 ) ;
#1502 = CARTESIAN_POINT ( 'NONE',  ( -299.8611223228758149, 3.740497495074990297E-15, 439.6443911606511392 ) ) ;
#1503 = CARTESIAN_POINT ( 'NONE',  ( 16.26935751051944479, 3.252606517456513302E-16, 140.3055424402290896 ) ) ;
#1504 = AXIS2_PLACEMENT_3D ( 'NONE', #1027, #4333, #536 ) ;
#1505 = ORIENTED_EDGE ( 'NONE', *, *, #1663, .F. ) ;
#1506 = CARTESIAN_POINT ( 'NONE',  ( -367.0882437885064746, 25.00000000000018474, 297.8351940652706276 ) ) ;
#1507 = ORIENTED_EDGE ( 'NONE', *, *, #5021, .F. ) ;
#1508 = AXIS2_PLACEMENT_3D ( 'NONE', #4653, #4245, #4981 ) ;
#1509 = DIRECTION ( 'NONE',  ( -5.551115123125772841E-17, 1.848892746611743135E-31, 1.000000000000000000 ) ) ;
#1510 = DIRECTION ( 'NONE',  ( -0.01527226085271972227, -2.080004339938201146E-31, -0.9998833722232041143 ) ) ;
#1511 = CIRCLE ( 'NONE', #3716, 21.00000000000012790 ) ;
#1512 = ORIENTED_EDGE ( 'NONE', *, *, #4796, .F. ) ;
#1513 = EDGE_CURVE ( 'NONE', #4212, #4831, #612, .T. ) ;
#1514 = VECTOR ( 'NONE', #1039, 1000.000000000000000 ) ;
#1515 = AXIS2_PLACEMENT_3D ( 'NONE', #3770, #4, #4625 ) ;
#1516 = ORIENTED_EDGE ( 'NONE', *, *, #2075, .F. ) ;
#1517 = DIRECTION ( 'NONE',  ( 0.4205749795070158337, 0.9072577839912276954, 0.000000000000000000 ) ) ;
#1518 = CARTESIAN_POINT ( 'NONE',  ( 113.4038502097781276, 0.000000000000000000, 172.0544138201894668 ) ) ;
#1519 = DIRECTION ( 'NONE',  ( -0.9955873536034883786, 5.498529991225532086E-31, -0.09383933793885522456 ) ) ;
#1520 = FACE_OUTER_BOUND ( 'NONE', #1417, .T. ) ;
#1521=STYLED_ITEM('',(#5451),#4977);
#1522 = AXIS2_PLACEMENT_3D ( 'NONE', #1614, #1638, #3330 ) ;
#1523 = CARTESIAN_POINT ( 'NONE',  ( 133.9714219172562366, 80.45434506795679397, -26.84924240491753977 ) ) ;
#1524 = ORIENTED_EDGE ( 'NONE', *, *, #1692, .T. ) ;
#1525 = LINE ( 'NONE', #2793, #4101 ) ;
#1526 = DIRECTION ( 'NONE',  ( -5.551115123125772841E-17, 1.848892746611743135E-31, 1.000000000000000000 ) ) ;
#1527 = AXIS2_PLACEMENT_3D ( 'NONE', #1320, #754, #2465 ) ;
#1528 = CARTESIAN_POINT ( 'NONE',  ( -351.5485029915759583, 2.222614453595284090E-15, 177.1955551554592603 ) ) ;
#1529 = DIRECTION ( 'NONE',  ( -0.09383933793885537722, 2.626968444144180508E-31, 0.9955873536034883786 ) ) ;
#1530 = AXIS2_PLACEMENT_3D ( 'NONE', #1395, #1824, #2217 ) ;
#1531 = DIRECTION ( 'NONE',  ( -1.000000000000000000, 0.000000000000000000, 0.000000000000000000 ) ) ;
#1532 = CIRCLE ( 'NONE', #652, 4.382543221487789076 ) ;
#1533 = AXIS2_PLACEMENT_3D ( 'NONE', #3128, #4792, #2245 ) ;
#1534 = EDGE_CURVE ( 'NONE', #483, #3766, #4570, .T. ) ;
#1535 = EDGE_CURVE ( 'NONE', #4186, #606, #3442, .T. ) ;
#1536 = FACE_OUTER_BOUND ( 'NONE', #1902, .T. ) ;
#1537 = CARTESIAN_POINT ( 'NONE',  ( -107.0991749147297014, 25.00000000000018474, 535.0680222229608489 ) ) ;
#1538 = CARTESIAN_POINT ( 'NONE',  ( -36.58361131987999926, -24.99999999999981881, 532.6725316595209279 ) ) ;
#1539 = DIRECTION ( 'NONE',  ( 1.000000000000000000, 0.000000000000000000, 5.551115123125782702E-17 ) ) ;
#1540 = ADVANCED_FACE ( 'NONE', ( #4732, #3825 ), #876, .T. ) ;
#1541 = EDGE_CURVE ( 'NONE', #2151, #1807, #5073, .T. ) ;
#1542 = PRODUCT_DEFINITION_FORMATION_WITH_SPECIFIED_SOURCE ( 'ANY', '', #2460, .NOT_KNOWN. ) ;
#1543 = ORIENTED_EDGE ( 'NONE', *, *, #3666, .F. ) ;
#1544 = CARTESIAN_POINT ( 'NONE',  ( -0.4023372602832280820, 25.00000000000018474, 421.4664991283991640 ) ) ;
#1545 = ORIENTED_EDGE ( 'NONE', *, *, #5330, .F. ) ;
#1546 = DIRECTION ( 'NONE',  ( 0.09383933793885568253, -2.673190762809473730E-31, -0.9955873536034882676 ) ) ;
#1547 = CARTESIAN_POINT ( 'NONE',  ( -346.0119820531830328, 0.000000000000000000, 118.4559012928528858 ) ) ;
#1548 = EDGE_LOOP ( 'NONE', ( #627, #510, #4173 ) ) ;
#1549 = UNCERTAINTY_MEASURE_WITH_UNIT (LENGTH_MEASURE( 1.000000000000000082E-05 ), #1806, 'distance_accuracy_value', 'NONE');
#1550 = ORIENTED_EDGE ( 'NONE', *, *, #2774, .T. ) ;
#1551 = CARTESIAN_POINT ( 'NONE',  ( -84.02857808274400497, -39.54565493204319893, -11.99999999999984368 ) ) ;
#1552 = FACE_OUTER_BOUND ( 'NONE', #3657, .T. ) ;
#1553 = DIRECTION ( 'NONE',  ( 1.000000000000000000, 0.000000000000000000, 5.551115123125777155E-17 ) ) ;
#1554 = CARTESIAN_POINT ( 'NONE',  ( -84.02857808274407603, 84.45434506795682239, -11.99999999999995559 ) ) ;
#1555 = DIRECTION ( 'NONE',  ( -2.523234146875361914E-16, -1.000000000000000000, -1.456973175402238023E-31 ) ) ;
#1556 = ORIENTED_EDGE ( 'NONE', *, *, #3185, .T. ) ;
#1557 = CARTESIAN_POINT ( 'NONE',  ( -351.7361816674535362, 5.421010862427522170E-17, 179.1867298626658283 ) ) ;
#1558 = DIRECTION ( 'NONE',  ( -5.551115123125772841E-17, 1.848892746611743135E-31, 1.000000000000000000 ) ) ;
#1559 = DIRECTION ( 'NONE',  ( 0.05689159511111528678, 0.000000000000000000, -0.9983803615885644689 ) ) ;
#1560 = CARTESIAN_POINT ( 'NONE',  ( -334.2354697480813002, 2.276824562219556945E-15, 40.21575531256979019 ) ) ;
#1561 = AXIS2_PLACEMENT_3D ( 'NONE', #3367, #2976, #4600 ) ;
#1562 = AXIS2_PLACEMENT_3D ( 'NONE', #1455, #5135, #2693 ) ;
#1563 = DIRECTION ( 'NONE',  ( -0.09383933793885568253, 2.673190762809473730E-31, 0.9955873536034882676 ) ) ;
#1564 = CARTESIAN_POINT ( 'NONE',  ( -213.0979982360508416, 24.99999999999997158, 511.7519955242232754 ) ) ;
#1565 = EDGE_CURVE ( 'NONE', #911, #4329, #4225, .T. ) ;
#1566 = CARTESIAN_POINT ( 'NONE',  ( -80.60298687151718866, -24.99999999999981881, 555.2885198911441194 ) ) ;
#1567 = ORIENTED_EDGE ( 'NONE', *, *, #567, .F. ) ;
#1568 = CARTESIAN_POINT ( 'NONE',  ( 11.65205807320727871, 25.00000000000018474, 340.0738060255407049 ) ) ;
#1569 = VERTEX_POINT ( 'NONE', #2619 ) ;
#1570 = CIRCLE ( 'NONE', #163, 27.50000000000126121 ) ;
#1571 = LINE ( 'NONE', #3642, #3907 ) ;
#1572 = CARTESIAN_POINT ( 'NONE',  ( -80.02857808274410445, -21.54565493204321669, -9.999999999999953815 ) ) ;
#1573 = ORIENTED_EDGE ( 'NONE', *, *, #4793, .T. ) ;
#1574 = VERTEX_POINT ( 'NONE', #1694 ) ;
#1575 = DIRECTION ( 'NONE',  ( 0.9955873536034882676, -5.499791016784056700E-31, 0.09383933793885550212 ) ) ;
#1576 = DIRECTION ( 'NONE',  ( -1.000000000000000000, 0.000000000000000000, -8.260587980841909197E-17 ) ) ;
#1577 = CARTESIAN_POINT ( 'NONE',  ( -98.02857808274411866, -25.54565493204307813, -11.99999999999995559 ) ) ;
#1578 = CYLINDRICAL_SURFACE ( 'NONE', #3372, 21.00000000000124700 ) ;
#1579 = FACE_OUTER_BOUND ( 'NONE', #1212, .T. ) ;
#1580 = ORIENTED_EDGE ( 'NONE', *, *, #2177, .F. ) ;
#1581 = CARTESIAN_POINT ( 'NONE',  ( 133.9714219172562366, 80.45434506795679397, -26.84924240491753977 ) ) ;
#1582 = CARTESIAN_POINT ( 'NONE',  ( -364.1439395362591540, 2.222614453595284090E-15, 237.2787335496894343 ) ) ;
#1583 = DIRECTION ( 'NONE',  ( -0.9955873536034882676, 5.484003909441380272E-31, -0.09383933793885536334 ) ) ;
#1584 = CARTESIAN_POINT ( 'NONE',  ( -84.02857808274413287, 84.45434506795682239, -5.551115123125782702E-14 ) ) ;
#1585 = AXIS2_PLACEMENT_3D ( 'NONE', #1956, #362, #2479 ) ;
#1586 = DIRECTION ( 'NONE',  ( 0.09383933793885568253, -2.673190762809473730E-31, -0.9955873536034882676 ) ) ;
#1587 = CARTESIAN_POINT ( 'NONE',  ( -198.3455225866221667, 24.99999999999997158, 518.3576047634796851 ) ) ;
#1588 = ITEM_DEFINED_TRANSFORMATION ( 'NONE', 'NONE', #2156,  #2926 ) ;
#1589 = CARTESIAN_POINT ( 'NONE',  ( -156.9923520473269321, 0.000000000000000000, 556.8176423728721147 ) ) ;
#1590 = ORIENTED_EDGE ( 'NONE', *, *, #4050, .F. ) ;
#1591 = CARTESIAN_POINT ( 'NONE',  ( -63.04765821498167355, 25.00000000000018474, 521.0401840782875524 ) ) ;
#1592 = ORIENTED_EDGE ( 'NONE', *, *, #1221, .T. ) ;
#1593 = DIRECTION ( 'NONE',  ( 0.09383933793885537722, -2.626968444144180508E-31, -0.9955873536034883786 ) ) ;
#1594 = FACE_OUTER_BOUND ( 'NONE', #4741, .T. ) ;
#1595 = AXIS2_PLACEMENT_3D ( 'NONE', #1145, #3602, #1088 ) ;
#1596 = VERTEX_POINT ( 'NONE', #3787 ) ;
#1597 = ADVANCED_FACE ( 'NONE', ( #4618 ), #3767, .T. ) ;
#1598 = ORIENTED_EDGE ( 'NONE', *, *, #1060, .T. ) ;
#1599 = DIRECTION ( 'NONE',  ( 0.09383933793885568253, -2.673190762809473730E-31, -0.9955873536034882676 ) ) ;
#1600 = DIRECTION ( 'NONE',  ( -0.9955873536034882676, 5.273458392682099492E-31, -0.09383933793885600172 ) ) ;
#1601 = EDGE_CURVE ( 'NONE', #4644, #3314, #81, .T. ) ;
#1602 = FACE_OUTER_BOUND ( 'NONE', #1128, .T. ) ;
#1603 = CARTESIAN_POINT ( 'NONE',  ( -98.02857808274411866, -25.54565493204307813, -11.99999999999995559 ) ) ;
#1604 = EDGE_CURVE ( 'NONE', #3069, #5397, #106, .T. ) ;
#1605 = EDGE_CURVE ( 'NONE', #2877, #3068, #4292, .T. ) ;
#1606 = CARTESIAN_POINT ( 'NONE',  ( 133.9714219172562650, 80.45434506795683660, -2.000000000000001776 ) ) ;
#1607 = VERTEX_POINT ( 'NONE', #23 ) ;
#1608 = ORIENTED_EDGE ( 'NONE', *, *, #3563, .F. ) ;
#1609 = FACE_OUTER_BOUND ( 'NONE', #4336, .T. ) ;
#1610 = CARTESIAN_POINT ( 'NONE',  ( -354.3266237013149862, 5.421010862427522170E-17, 381.2801272015580025 ) ) ;
#1611 = DIRECTION ( 'NONE',  ( -0.4205749795070160557, 0.9072577839912276954, 5.551115123125780853E-17 ) ) ;
#1612 = AXIS2_PLACEMENT_3D ( 'NONE', #3970, #2266, #1771 ) ;
#1613=STYLED_ITEM('',(#5451),#3136);
#1614 = CARTESIAN_POINT ( 'NONE',  ( 29.23877717791895492, 0.000000000000000000, 67.09613410133256650 ) ) ;
#1615 = AXIS2_PLACEMENT_3D ( 'NONE', #3562, #663, #4833 ) ;
#1616 = VECTOR ( 'NONE', #912, 1000.000000000000000 ) ;
#1617 = CARTESIAN_POINT ( 'NONE',  ( 133.9714219172562366, -21.54565493204319182, -26.84924240491753977 ) ) ;
#1618 = CARTESIAN_POINT ( 'NONE',  ( -52.92425795465503313, 25.00000000000018474, 513.6488213284155790 ) ) ;
#1619 = CARTESIAN_POINT ( 'NONE',  ( -264.1404626571541598, -25.00000000000003197, 511.7445549721641100 ) ) ;
#1620 = VECTOR ( 'NONE', #3761, 1000.000000000000000 ) ;
#1621 = CIRCLE ( 'NONE', #1183, 4.382543221487789076 ) ;
#1622 = VERTEX_POINT ( 'NONE', #3476 ) ;
#1623 = ORIENTED_EDGE ( 'NONE', *, *, #3398, .T. ) ;
#1624 = ADVANCED_FACE ( 'NONE', ( #4237, #1724 ), #3391, .F. ) ;
#1625 = CARTESIAN_POINT ( 'NONE',  ( 135.7157751673381085, -16.59391465826787027, -9.999999999999953815 ) ) ;
#1626 = CYLINDRICAL_SURFACE ( 'NONE', #2411, 14.00000000000002665 ) ;
#1627 = ORIENTED_EDGE ( 'NONE', *, *, #1787, .F. ) ;
#1628 =( LENGTH_UNIT ( ) NAMED_UNIT ( * ) SI_UNIT ( .MILLI., .METRE. ) );
#1629 = FACE_OUTER_BOUND ( 'NONE', #406, .T. ) ;
#1630 = CARTESIAN_POINT ( 'NONE',  ( 135.9827310413679413, -14.99999999999998579, 131.6034880481681171 ) ) ;
#1631 = DIRECTION ( 'NONE',  ( 5.551115123125772841E-17, -1.848892746611743135E-31, -1.000000000000000000 ) ) ;
#1632 = ORIENTED_EDGE ( 'NONE', *, *, #965, .T. ) ;
#1633 = EDGE_LOOP ( 'NONE', ( #2754, #1391, #4723 ) ) ;
#1634 = DIRECTION ( 'NONE',  ( -0.9998833722232040033, 6.797399803719615819E-31, 0.01527226085271964420 ) ) ;
#1635 = EDGE_CURVE ( 'NONE', #4435, #2041, #2505, .T. ) ;
#1636 = FACE_OUTER_BOUND ( 'NONE', #5316, .T. ) ;
#1637 = LINE ( 'NONE', #1743, #213 ) ;
#1638 = DIRECTION ( 'NONE',  ( 0.000000000000000000, 1.000000000000000000, 0.000000000000000000 ) ) ;
#1639 = CARTESIAN_POINT ( 'NONE',  ( -86.97194166595129161, 3.740497495074990297E-15, 531.0655262460708173 ) ) ;
#1640 = CARTESIAN_POINT ( 'NONE',  ( -13.17877320795229856, 25.00000000000000355, 47.33401081801169141 ) ) ;
#1641 = CARTESIAN_POINT ( 'NONE',  ( 35.78913469918423829, 0.000000000000000000, 310.6402212931345161 ) ) ;
#1642 = ORIENTED_EDGE ( 'NONE', *, *, #2200, .T. ) ;
#1643 = CIRCLE ( 'NONE', #3594, 2.000000000000001776 ) ;
#1644 = CARTESIAN_POINT ( 'NONE',  ( -77.37696704867106234, 84.98551036222526989, -9.999999999999953815 ) ) ;
#1645 = FACE_OUTER_BOUND ( 'NONE', #2543, .T. ) ;
#1646 = AXIS2_PLACEMENT_3D ( 'NONE', #4564, #1586, #789 ) ;
#1647 = ORIENTED_EDGE ( 'NONE', *, *, #2888, .T. ) ;
#1648 = VERTEX_POINT ( 'NONE', #2945 ) ;
#1649 = CARTESIAN_POINT ( 'NONE',  ( 132.2270686671743931, -26.49739520581860575, -11.99999999999990052 ) ) ;
#1650 = CARTESIAN_POINT ( 'NONE',  ( -84.02857808274407603, 84.45434506795682239, -11.99999999999995559 ) ) ;
#1651 = DIRECTION ( 'NONE',  ( 5.551115123125772841E-17, -1.848892746611743135E-31, -1.000000000000000000 ) ) ;
#1652 = DIRECTION ( 'NONE',  ( 0.9998833722232041143, -6.779273404243020281E-31, -0.01527226085271993043 ) ) ;
#1653 = EDGE_CURVE ( 'NONE', #2041, #4297, #3909, .T. ) ;
#1654 = VERTEX_POINT ( 'NONE', #937 ) ;
#1655 = ORIENTED_EDGE ( 'NONE', *, *, #1834, .F. ) ;
#1656 = DIRECTION ( 'NONE',  ( 0.000000000000000000, 1.000000000000000000, 0.000000000000000000 ) ) ;
#1657 = DIRECTION ( 'NONE',  ( 0.000000000000000000, 1.000000000000000000, 0.000000000000000000 ) ) ;
#1658 = CARTESIAN_POINT ( 'NONE',  ( -17.84624325233685127, 4.358724120770097062E-15, 36.40401889739442254 ) ) ;
#1659 = FACE_OUTER_BOUND ( 'NONE', #1345, .T. ) ;
#1660 = CARTESIAN_POINT ( 'NONE',  ( -320.3751800289425091, 5.421010862425815642E-17, 182.1426690077398689 ) ) ;
#1661 = CARTESIAN_POINT ( 'NONE',  ( -342.0244061588616091, 3.740497495074990297E-15, 297.0039604601894894 ) ) ;
#1662 = FACE_OUTER_BOUND ( 'NONE', #665, .T. ) ;
#1663 = EDGE_CURVE ( 'NONE', #4330, #1984, #5101, .T. ) ;
#1664 = EDGE_CURVE ( 'NONE', #4404, #1665, #1393, .T. ) ;
#1665 = VERTEX_POINT ( 'NONE', #2147 ) ;
#1666 = DIRECTION ( 'NONE',  ( -0.9955873536034882676, 5.436595176548168253E-31, -0.09383933793885573804 ) ) ;
#1667 = DIRECTION ( 'NONE',  ( 0.000000000000000000, 1.000000000000000000, 0.000000000000000000 ) ) ;
#1668 = ORIENTED_EDGE ( 'NONE', *, *, #993, .T. ) ;
#1669 = DIRECTION ( 'NONE',  ( -1.261617073437686134E-16, 1.000000000000000000, 1.232595164407830946E-31 ) ) ;
#1670 = CARTESIAN_POINT ( 'NONE',  ( -353.5191290882918338, 0.000000000000000000, 198.1028895811327573 ) ) ;
#1671 = DIRECTION ( 'NONE',  ( -0.9955873536034882676, 5.498529991225543472E-31, -0.09383933793885566865 ) ) ;
#1672 = CARTESIAN_POINT ( 'NONE',  ( -84.02857808274403340, 98.45434506795682239, -5.551115123125782702E-14 ) ) ;
#1673 = CIRCLE ( 'NONE', #3009, 49.99999999999996447 ) ;
#1674 = EDGE_CURVE ( 'NONE', #3692, #486, #5136, .T. ) ;
#1675 = EDGE_LOOP ( 'NONE', ( #315, #4754, #4352, #5255 ) ) ;
#1676 = VERTEX_POINT ( 'NONE', #3874 ) ;
#1677 = VECTOR ( 'NONE', #1387, 1000.000000000000000 ) ;
#1678 = VERTEX_POINT ( 'NONE', #1260 ) ;
#1679 = CARTESIAN_POINT ( 'NONE',  ( -377.2791443537555551, 3.911847525938623293E-15, 114.5043747941758596 ) ) ;
#1680 = CARTESIAN_POINT ( 'NONE',  ( 0.000000000000000000, 80.00000000000000000, 0.000000000000000000 ) ) ;
#1681 = FACE_BOUND ( 'NONE', #3612, .T. ) ;
#1682 = CIRCLE ( 'NONE', #4936, 1.000000000000000888 ) ;
#1683 = DIRECTION ( 'NONE',  ( -0.9955873536034882676, 0.000000000000000000, -0.09383933793885600172 ) ) ;
#1684 = VECTOR ( 'NONE', #4117, 1000.000000000000000 ) ;
#1685 = CARTESIAN_POINT ( 'NONE',  ( -66.30461487616335603, 0.000000000000000000, 161.8139267001887447 ) ) ;
#1686 = CARTESIAN_POINT ( 'NONE',  ( -23.53079058812344471, -24.99999999999981881, 476.4235034963351154 ) ) ;
#1687 = DIRECTION ( 'NONE',  ( 0.9072577839912275843, 0.4205749795070160002, 1.110223024625155801E-16 ) ) ;
#1688 = AXIS2_PLACEMENT_3D ( 'NONE', #1874, #1326, #4303 ) ;
#1689 = EDGE_CURVE ( 'NONE', #3205, #2195, #5157, .T. ) ;
#1690 = VECTOR ( 'NONE', #3423, 1000.000000000000000 ) ;
#1691 = EDGE_LOOP ( 'NONE', ( #4106, #1608, #1655, #2367 ) ) ;
#1692 = EDGE_CURVE ( 'NONE', #463, #276, #1405, .T. ) ;
#1693 = ORIENTED_EDGE ( 'NONE', *, *, #3729, .F. ) ;
#1694 = CARTESIAN_POINT ( 'NONE',  ( -376.3773963380906480, 1.662953840130941270E-29, 115.5938014857176768 ) ) ;
#1695 = AXIS2_PLACEMENT_3D ( 'NONE', #4997, #3393, #1189 ) ;
#1696 = EDGE_CURVE ( 'NONE', #4078, #3095, #1114, .T. ) ;
#1697 = CIRCLE ( 'NONE', #648, 4.382543221487789964 ) ;
#1698 = AXIS2_PLACEMENT_3D ( 'NONE', #3408, #407, #4198 ) ;
#1699 = VECTOR ( 'NONE', #1297, 999.9999999999998863 ) ;
#1700 = ORIENTED_EDGE ( 'NONE', *, *, #334, .T. ) ;
#1701 = CARTESIAN_POINT ( 'NONE',  ( -348.7799179161582970, 2.813531315051574489E-15, 101.1196613272007738 ) ) ;
#1702 = VECTOR ( 'NONE', #1611, 999.9999999999998863 ) ;
#1703 = DIRECTION ( 'NONE',  ( 0.09383933793885568253, -2.673190762809473730E-31, -0.9955873536034882676 ) ) ;
#1704 = PRODUCT ( 'Stainless Steel Outer Shield Cover', 'Stainless Steel Outer Shield Cover', '', ( #5183 ) ) ;
#1705 = LINE ( 'NONE', #2094, #3463 ) ;
#1706 = CARTESIAN_POINT ( 'NONE',  ( -344.1351952944061168, 5.421010862427522170E-17, 98.54415422078321285 ) ) ;
#1707 = DIRECTION ( 'NONE',  ( -0.9955873536034882676, 5.498529991225538217E-31, -0.09383933793885536334 ) ) ;
#1708 = CARTESIAN_POINT ( 'NONE',  ( 131.3198108831832656, 84.98551036222518462, -10.00000000000000888 ) ) ;
#1709 = EDGE_LOOP ( 'NONE', ( #3945, #366 ) ) ;
#1710 = ORIENTED_EDGE ( 'NONE', *, *, #357, .T. ) ;
#1711 = ORIENTED_EDGE ( 'NONE', *, *, #1203, .T. ) ;
#1712 = DIRECTION ( 'NONE',  ( 0.09383933793885568253, -2.673190762809473730E-31, -0.9955873536034882676 ) ) ;
#1713 = CARTESIAN_POINT ( 'NONE',  ( -80.02857808274401918, 80.45434506795689344, -12.00000000000001066 ) ) ;
#1714 = DIRECTION ( 'NONE',  ( -0.09383933793885536334, 2.626968444144180070E-31, 0.9955873536034882676 ) ) ;
#1715 = SURFACE_STYLE_USAGE ( .BOTH. , #4335 ) ;
#1716 = ORIENTED_EDGE ( 'NONE', *, *, #1696, .F. ) ;
#1717 = ADVANCED_FACE ( 'NONE', ( #4804 ), #2437, .T. ) ;
#1718 = CARTESIAN_POINT ( 'NONE',  ( -74.77857808274418971, -21.54565493204320248, -2.000000000000001332 ) ) ;
#1719 = CARTESIAN_POINT ( 'NONE',  ( -167.9289969670494997, 3.740497495074990297E-15, 528.5729890193238134 ) ) ;
#1720 = CARTESIAN_POINT ( 'NONE',  ( 29.23877717791899400, 15.00000000000001421, 17.09613410133265532 ) ) ;
#1721 = ORIENTED_EDGE ( 'NONE', *, *, #1601, .T. ) ;
#1722 = EDGE_CURVE ( 'NONE', #3703, #1751, #715, .T. ) ;
#1723 = ORIENTED_EDGE ( 'NONE', *, *, #720, .T. ) ;
#1724 = FACE_BOUND ( 'NONE', #4138, .T. ) ;
#1725 =( LENGTH_UNIT ( ) NAMED_UNIT ( * ) SI_UNIT ( .MILLI., .METRE. ) );
#1726 = AXIS2_PLACEMENT_3D ( 'NONE', #593, #1013, #1474 ) ;
#1727 = PLANE ( 'NONE',  #1445 ) ;
#1728 = VERTEX_POINT ( 'NONE', #4123 ) ;
#1729 = DIRECTION ( 'NONE',  ( 0.09383933793885537722, -2.626968444144180508E-31, -0.9955873536034883786 ) ) ;
#1730 = AXIS2_PLACEMENT_3D ( 'NONE', #3109, #2299, #2715 ) ;
#1731 = CARTESIAN_POINT ( 'NONE',  ( -342.9618789639491752, 2.813531315051557923E-15, 39.39324540378412109 ) ) ;
#1732 = CARTESIAN_POINT ( 'NONE',  ( -121.8424039466566313, 3.794707603699265519E-15, 535.4314447305365547 ) ) ;
#1733 = PRESENTATION_STYLE_ASSIGNMENT (( #64 ) ) ;
#1734 = DIRECTION ( 'NONE',  ( -6.938893903907233308E-17, 0.000000000000000000, -1.000000000000000000 ) ) ;
#1735 = DIRECTION ( 'NONE',  ( 0.000000000000000000, 1.000000000000000000, 0.000000000000000000 ) ) ;
#1736 = EDGE_CURVE ( 'NONE', #1160, #4218, #729, .T. ) ;
#1737 = VECTOR ( 'NONE', #1918, 1000.000000000000114 ) ;
#1738 = VERTEX_POINT ( 'NONE', #3683 ) ;
#1739 = ORIENTED_EDGE ( 'NONE', *, *, #2854, .F. ) ;
#1740 = ORIENTED_EDGE ( 'NONE', *, *, #2176, .T. ) ;
#1741 = DIRECTION ( 'NONE',  ( 5.551115123125772841E-17, -1.848892746611743354E-31, -1.000000000000000000 ) ) ;
#1742 = CARTESIAN_POINT ( 'NONE',  ( 119.2387771779189478, 0.000000000000000000, 167.0961341013325523 ) ) ;
#1743 = CARTESIAN_POINT ( 'NONE',  ( -74.02857808274416129, -21.54565493204321669, -2.000000000000001332 ) ) ;
#1744 = DIRECTION ( 'NONE',  ( 1.261617073437686134E-16, -1.000000000000000000, -1.232595164407830946E-31 ) ) ;
#1745 = ORIENTED_EDGE ( 'NONE', *, *, #3733, .T. ) ;
#1746 = EDGE_CURVE ( 'NONE', #1423, #3805, #352, .T. ) ;
#1747 = LINE ( 'NONE', #1685, #5341 ) ;
#1748 = CARTESIAN_POINT ( 'NONE',  ( -86.97194166595193110, -24.99999999999981881, 531.0655262460722952 ) ) ;
#1749 = LINE ( 'NONE', #2198, #3473 ) ;
#1750 = ORIENTED_EDGE ( 'NONE', *, *, #166, .T. ) ;
#1751 = VERTEX_POINT ( 'NONE', #4036 ) ;
#1752 = DIRECTION ( 'NONE',  ( -0.9955873536034882676, 5.452307672560245432E-31, -0.09383933793885568253 ) ) ;
#1753 = EDGE_CURVE ( 'NONE', #907, #2587, #3276, .T. ) ;
#1754 = ORIENTED_EDGE ( 'NONE', *, *, #2852, .T. ) ;
#1755 = CARTESIAN_POINT ( 'NONE',  ( -80.60298687151650654, 2.222614453595284090E-15, 555.2885198911399129 ) ) ;
#1756 = APPLICATION_CONTEXT ( 'automotive_design' ) ;
#1757 = VECTOR ( 'NONE', #498, 1000.000000000000000 ) ;
#1758 = DIRECTION ( 'NONE',  ( 0.4205749795070160557, -0.9072577839912276954, -5.551115123125780853E-17 ) ) ;
#1759 = CARTESIAN_POINT ( 'NONE',  ( -213.0979982360508416, -25.00000000000003197, 511.7519955242232754 ) ) ;
#1760 = CARTESIAN_POINT ( 'NONE',  ( -333.8864425577414181, 2.759321206427298478E-15, 102.5234496157762578 ) ) ;
#1761 = CARTESIAN_POINT ( 'NONE',  ( -324.0724149101815783, 5.421010862424517719E-17, 109.4750664999304348 ) ) ;
#1762 = ORIENTED_EDGE ( 'NONE', *, *, #166, .F. ) ;
#1763 = ORIENTED_EDGE ( 'NONE', *, *, #4567, .F. ) ;
#1764 = ADVANCED_FACE ( 'NONE', ( #5286 ), #3338, .F. ) ;
#1765 = ADVANCED_FACE ( 'NONE', ( #1173 ), #4445, .T. ) ;
#1766 = ORIENTED_EDGE ( 'NONE', *, *, #1870, .T. ) ;
#1767 = CIRCLE ( 'NONE', #5369, 17.00000000000009948 ) ;
#1768 = CARTESIAN_POINT ( 'NONE',  ( -374.4800609688232953, 1.553907686679738498E-29, 116.7770675151984392 ) ) ;
#1769 = ADVANCED_FACE ( 'NONE', ( #4904 ), #3190, .T. ) ;
#1770 = DIRECTION ( 'NONE',  ( -0.4205749795070160557, 0.9072577839912276954, 5.551115123125780853E-17 ) ) ;
#1771 = DIRECTION ( 'NONE',  ( -1.000000000000000000, 0.000000000000000000, 0.000000000000000000 ) ) ;
#1772 = ADVANCED_FACE ( 'NONE', ( #785 ), #3221, .F. ) ;
#1773 = CARTESIAN_POINT ( 'NONE',  ( 133.9714219172562650, 80.45434506795683660, -2.000000000000001776 ) ) ;
#1774 = EDGE_LOOP ( 'NONE', ( #2764, #625, #4453, #2047 ) ) ;
#1775 = AXIS2_PLACEMENT_3D ( 'NONE', #949, #1051, #5120 ) ;
#1776 = EDGE_CURVE ( 'NONE', #4528, #3229, #1494, .T. ) ;
#1777 = CARTESIAN_POINT ( 'NONE',  ( 151.9714219172563219, 84.45434506795677976, -5.551115123125782702E-14 ) ) ;
#1778 = CARTESIAN_POINT ( 'NONE',  ( -63.04765821500757284, -24.99999999999981881, 521.0401840782880072 ) ) ;
#1779 = DIRECTION ( 'NONE',  ( -0.9955873536034884896, 0.000000000000000000, -0.09383933793885443353 ) ) ;
#1780 = ORIENTED_EDGE ( 'NONE', *, *, #3960, .T. ) ;
#1781 = VECTOR ( 'NONE', #2974, 1000.000000000000000 ) ;
#1782 = AXIS2_PLACEMENT_3D ( 'NONE', #3793, #2919, #344 ) ;
#1783 = ORIENTED_EDGE ( 'NONE', *, *, #4151, .F. ) ;
#1784 = CARTESIAN_POINT ( 'NONE',  ( -78.28422483266226095, 85.40608534173227895, -10.00000000000006395 ) ) ;
#1785 = AXIS2_PLACEMENT_3D ( 'NONE', #1491, #2815, #2846 ) ;
#1786 =( GEOMETRIC_REPRESENTATION_CONTEXT ( 3 ) GLOBAL_UNCERTAINTY_ASSIGNED_CONTEXT ( ( #3590 ) ) GLOBAL_UNIT_ASSIGNED_CONTEXT ( ( #5203, #2686, #5280 ) ) REPRESENTATION_CONTEXT ( 'NONE', 'WORKASPACE' ) );
#1787 = EDGE_CURVE ( 'NONE', #3984, #5060, #4324, .T. ) ;
#1788 = VERTEX_POINT ( 'NONE', #3247 ) ;
#1789 = CARTESIAN_POINT ( 'NONE',  ( -264.1404626571534777, 2.222614453595284090E-15, 511.7445549721628595 ) ) ;
#1790 = AXIS2_PLACEMENT_3D ( 'NONE', #3942, #193, #3532 ) ;
#1791 = CIRCLE ( 'NONE', #2672, 4.382543221487789076 ) ;
#1792 = CYLINDRICAL_SURFACE ( 'NONE', #905, 77.49999999999998579 ) ;
#1793 = CARTESIAN_POINT ( 'NONE',  ( -0.4023372603089575006, -24.99999999999981881, 421.4664991283988229 ) ) ;
#1794 = LINE ( 'NONE', #5266, #2481 ) ;
#1795 = CARTESIAN_POINT ( 'NONE',  ( 151.9714219172562935, 84.45434506795673713, -11.99999999999995559 ) ) ;
#1796 = VECTOR ( 'NONE', #313, 1000.000000000000114 ) ;
#1797 = VECTOR ( 'NONE', #211, 1000.000000000000000 ) ;
#1798 = AXIS2_PLACEMENT_3D ( 'NONE', #3324, #1277, #41 ) ;
#1799 = VERTEX_POINT ( 'NONE', #4847 ) ;
#1800 = ORIENTED_EDGE ( 'NONE', *, *, #5103, .T. ) ;
#1801 = ORIENTED_EDGE ( 'NONE', *, *, #330, .F. ) ;
#1802 = EDGE_CURVE ( 'NONE', #557, #1151, #2652, .T. ) ;
#1803 = FACE_OUTER_BOUND ( 'NONE', #3535, .T. ) ;
#1804 = DIRECTION ( 'NONE',  ( 0.09383933793885537722, -2.626968444144180508E-31, -0.9955873536034883786 ) ) ;
#1805 = DIRECTION ( 'NONE',  ( -0.9955873536034883786, 5.498529991225544347E-31, -0.09383933793885444741 ) ) ;
#1806 =( LENGTH_UNIT ( ) NAMED_UNIT ( * ) SI_UNIT ( .MILLI., .METRE. ) );
#1807 = VERTEX_POINT ( 'NONE', #1742 ) ;
#1808 = DIRECTION ( 'NONE',  ( 5.551115123125772841E-17, -1.848892746611743135E-31, -1.000000000000000000 ) ) ;
#1809 = CARTESIAN_POINT ( 'NONE',  ( -342.0244061588616091, -24.99999999999981881, 297.0039604601892620 ) ) ;
#1810 = FACE_OUTER_BOUND ( 'NONE', #2145, .T. ) ;
#1811 = CARTESIAN_POINT ( 'NONE',  ( -338.5986743560152377, 2.276824562219559311E-15, 39.80450035817695209 ) ) ;
#1812 = DIRECTION ( 'NONE',  ( -0.01527226085271972227, -2.080004339938201146E-31, -0.9998833722232041143 ) ) ;
#1813 = APPLICATION_PROTOCOL_DEFINITION ( 'draft international standard', 'automotive_design', 1998, #2817 ) ;
#1814 = VERTEX_POINT ( 'NONE', #926 ) ;
#1815 = CARTESIAN_POINT ( 'NONE',  ( 18.31346110193259946, 25.00000000000018474, 444.2932575970297648 ) ) ;
#1816 = ORIENTED_EDGE ( 'NONE', *, *, #2103, .F. ) ;
#1817 = AXIS2_PLACEMENT_3D ( 'NONE', #516, #155, #3521 ) ;
#1818 = PLANE ( 'NONE',  #2132 ) ;
#1819 = CARTESIAN_POINT ( 'NONE',  ( 36.66581985038869362, 3.252606517456513302E-16, 340.1662229844753256 ) ) ;
#1820 = LINE ( 'NONE', #3008, #2584 ) ;
#1821 = AXIS2_PLACEMENT_3D ( 'NONE', #3550, #957, #575 ) ;
#1822 = ORIENTED_EDGE ( 'NONE', *, *, #1198, .F. ) ;
#1823 = ORIENTED_EDGE ( 'NONE', *, *, #57, .F. ) ;
#1824 = DIRECTION ( 'NONE',  ( 0.09383933793885568253, -2.673190762809473730E-31, -0.9955873536034882676 ) ) ;
#1825 = CARTESIAN_POINT ( 'NONE',  ( -378.1397951484382816, 2.222614453595299078E-15, 155.6049743057346291 ) ) ;
#1826 = DIRECTION ( 'NONE',  ( -0.9955873536034883786, 5.498529991225525955E-31, -0.09383933793885444741 ) ) ;
#1827 = FACE_OUTER_BOUND ( 'NONE', #1304, .T. ) ;
#1828 = ORIENTED_EDGE ( 'NONE', *, *, #4993, .F. ) ;
#1829 = AXIS2_PLACEMENT_3D ( 'NONE', #2962, #2473, #1337 ) ;
#1830 = DIRECTION ( 'NONE',  ( 0.000000000000000000, -1.000000000000000000, 0.000000000000000000 ) ) ;
#1831 = CARTESIAN_POINT ( 'NONE',  ( 16.26935751051938439, -25.00000000000000355, 140.3055424402287770 ) ) ;
#1832 = DIRECTION ( 'NONE',  ( 1.000000000000000000, 0.000000000000000000, 0.000000000000000000 ) ) ;
#1833 =( BOUNDED_SURFACE ( )  B_SPLINE_SURFACE ( 3, 3, ( 
 ( #2179, #3086, #3962, #5218, #1460, #3038, #2641, #5107, #3509, #524, #2206, #1350, #551, #4376, #4709, #3852, #939, #83, #4296, #3481, #2622, #5164, #1755, #1407, #3876, #3914, #4753, #168, #1382, #1789, #110, #3062, #140, #992, #2256, #5138, #3143, #2669 ),
 ( #4734, #4806, #1868, #963, #4321, #189, #501, #3447, #2233, #1841, #2696, #1019, #1815, #4351, #578, #3938, #3529, #5186, #1429, #4785, #1043, #3116, #601, #3555, #2718, #1953, #4454, #277, #3691, #4912, #3640, #4107, #2804, #3256, #3669, #1506, #2366, #1185 ),
 ( #1152, #5326, #3230, #3282, #2336, #3992, #222, #1568, #4946, #3171, #338, #1544, #1067, #2746, #2831, #5268, #3204, #5355, #250, #1591, #660, #3611, #4399, #4865, #684, #4830, #2779, #4019, #4509, #626, #743, #4045, #1924, #1099, #5301, #4889, #1127, #2306 ),
 ( #1985, #4482, #707, #2393, #4077, #2426, #310, #1898, #2010, #3585, #5243, #1483, #4427, #4542, #2866, #768, #2454, #4130, #360, #1251, #3064, #2184, #3004, #1355, #1732, #503, #2598, #4017, #5265, #4736, #1896, #1502, #968, #2624, #113, #2302, #2644, #3199 ),
 ( #3608, #2333, #4677, #2157, #941, #916, #4396, #3426, #4273, #247, #3879, #1793, #1481, #622, #1065, #3169, #3855, #1921, #4243, #5142, #657, #4858, #2561, #5078, #4712, #1322, #3485, #87, #1759, #3450, #4301, #2741, #5110, #478, #3040, #3832, #527, #2210 ),
 ( #63, #1386, #3987, #218, #3583, #5240, #4828, #4424, #2035, #2887, #333, #1096, #3744, #1949, #2775, #1982, #3312, #4042, #1538, #5407, #2475, #2389, #1566, #4566, #4451, #680, #305, #2451, #4972, #1619, #2362, #2424, #4072, #2007, #273, #3689, #1123, #4503 ),
 ( #4910, #738, #3710, #791, #5353, #3636, #1641, #5295, #3227, #3665, #1210, #4886, #2800, #3336, #4155, #5324, #3253, #384, #4479, #704, #1150, #4127, #2061, #2828, #4105, #1589, #3279, #4941, #1180, #2864, #4540, #5381, #764, #358, #2964, #1256, #18, #2552 ) ),
 .UNSPECIFIED., .T., .F., .F. ) 
 B_SPLINE_SURFACE_WITH_KNOTS ( ( 4, 3, 4 ),
 ( 4, 2, 2, 2, 2, 2, 2, 2, 2, 2, 2, 2, 2, 2, 2, 2, 2, 2, 4 ),
 ( 0.000000000000000000, 0.5000000000000000000, 1.000000000000000000 ),
 ( 0.000000000000000000, 0.1028767157186024211, 0.2057534314372048423, 0.2571917892965060459, 0.3086301471558072773, 0.3600685050151084532, 0.4115068628744096846, 0.4558387458985032614, 0.4780046874105500776, 0.5001706289225968938, 0.5231687412733679876, 0.5461668536241390814, 0.5921630783256812691, 0.6381593030272234568, 0.6841555277287657555, 0.7631166457965743444, 0.8420777638643828222, 0.9210388819321914111, 1.000000000000000000 ),
 .UNSPECIFIED. ) 
 GEOMETRIC_REPRESENTATION_ITEM ( )  RATIONAL_B_SPLINE_SURFACE ( (
 ( 1.000000000000000000, 1.000000000000000000, 1.000000000000000000, 1.000000000000000000, 1.000000000000000000, 1.000000000000000000, 1.000000000000000000, 1.000000000000000000, 1.000000000000000000, 1.000000000000000000, 1.000000000000000000, 1.000000000000000000, 1.000000000000000000, 1.000000000000000000, 1.000000000000000000, 1.000000000000000000, 1.000000000000000000, 1.000000000000000000, 1.000000000000000000, 1.000000000000000000, 1.000000000000000000, 1.000000000000000000, 1.000000000000000000, 1.000000000000000000, 1.000000000000000000, 1.000000000000000000, 1.000000000000000000, 1.000000000000000000, 1.000000000000000000, 1.000000000000000000, 1.000000000000000000, 1.000000000000000000, 1.000000000000000000, 1.000000000000000000, 1.000000000000000000, 1.000000000000000000, 1.000000000000000000, 1.000000000000000000),
 ( 0.3333333333333333703, 0.3333333333333333703, 0.3333333333333333703, 0.3333333333333333703, 0.3333333333333333703, 0.3333333333333333703, 0.3333333333333333703, 0.3333333333333333703, 0.3333333333333333703, 0.3333333333333333703, 0.3333333333333333703, 0.3333333333333333703, 0.3333333333333333703, 0.3333333333333333703, 0.3333333333333333703, 0.3333333333333333703, 0.3333333333333333703, 0.3333333333333333703, 0.3333333333333333703, 0.3333333333333333703, 0.3333333333333333703, 0.3333333333333333703, 0.3333333333333333703, 0.3333333333333333703, 0.3333333333333333703, 0.3333333333333333703, 0.3333333333333333703, 0.3333333333333333703, 0.3333333333333333703, 0.3333333333333333703, 0.3333333333333333703, 0.3333333333333333703, 0.3333333333333333703, 0.3333333333333333703, 0.3333333333333333703, 0.3333333333333333703, 0.3333333333333333703, 0.3333333333333333703),
 ( 0.3333333333333333703, 0.3333333333333333703, 0.3333333333333333703, 0.3333333333333333703, 0.3333333333333333703, 0.3333333333333333703, 0.3333333333333333703, 0.3333333333333333703, 0.3333333333333333703, 0.3333333333333333703, 0.3333333333333333703, 0.3333333333333333703, 0.3333333333333333703, 0.3333333333333333703, 0.3333333333333333703, 0.3333333333333333703, 0.3333333333333333703, 0.3333333333333333703, 0.3333333333333333703, 0.3333333333333333703, 0.3333333333333333703, 0.3333333333333333703, 0.3333333333333333703, 0.3333333333333333703, 0.3333333333333333703, 0.3333333333333333703, 0.3333333333333333703, 0.3333333333333333703, 0.3333333333333333703, 0.3333333333333333703, 0.3333333333333333703, 0.3333333333333333703, 0.3333333333333333703, 0.3333333333333333703, 0.3333333333333333703, 0.3333333333333333703, 0.3333333333333333703, 0.3333333333333333703),
 ( 1.000000000000000000, 1.000000000000000000, 1.000000000000000000, 1.000000000000000000, 1.000000000000000000, 1.000000000000000000, 1.000000000000000000, 1.000000000000000000, 1.000000000000000000, 1.000000000000000000, 1.000000000000000000, 1.000000000000000000, 1.000000000000000000, 1.000000000000000000, 1.000000000000000000, 1.000000000000000000, 1.000000000000000000, 1.000000000000000000, 1.000000000000000000, 1.000000000000000000, 1.000000000000000000, 1.000000000000000000, 1.000000000000000000, 1.000000000000000000, 1.000000000000000000, 1.000000000000000000, 1.000000000000000000, 1.000000000000000000, 1.000000000000000000, 1.000000000000000000, 1.000000000000000000, 1.000000000000000000, 1.000000000000000000, 1.000000000000000000, 1.000000000000000000, 1.000000000000000000, 1.000000000000000000, 1.000000000000000000),
 ( 0.3333333333333333703, 0.3333333333333333703, 0.3333333333333333703, 0.3333333333333333703, 0.3333333333333333703, 0.3333333333333333703, 0.3333333333333333703, 0.3333333333333333703, 0.3333333333333333703, 0.3333333333333333703, 0.3333333333333333703, 0.3333333333333333703, 0.3333333333333333703, 0.3333333333333333703, 0.3333333333333333703, 0.3333333333333333703, 0.3333333333333333703, 0.3333333333333333703, 0.3333333333333333703, 0.3333333333333333703, 0.3333333333333333703, 0.3333333333333333703, 0.3333333333333333703, 0.3333333333333333703, 0.3333333333333333703, 0.3333333333333333703, 0.3333333333333333703, 0.3333333333333333703, 0.3333333333333333703, 0.3333333333333333703, 0.3333333333333333703, 0.3333333333333333703, 0.3333333333333333703, 0.3333333333333333703, 0.3333333333333333703, 0.3333333333333333703, 0.3333333333333333703, 0.3333333333333333703),
 ( 0.3333333333333333703, 0.3333333333333333703, 0.3333333333333333703, 0.3333333333333333703, 0.3333333333333333703, 0.3333333333333333703, 0.3333333333333333703, 0.3333333333333333703, 0.3333333333333333703, 0.3333333333333333703, 0.3333333333333333703, 0.3333333333333333703, 0.3333333333333333703, 0.3333333333333333703, 0.3333333333333333703, 0.3333333333333333703, 0.3333333333333333703, 0.3333333333333333703, 0.3333333333333333703, 0.3333333333333333703, 0.3333333333333333703, 0.3333333333333333703, 0.3333333333333333703, 0.3333333333333333703, 0.3333333333333333703, 0.3333333333333333703, 0.3333333333333333703, 0.3333333333333333703, 0.3333333333333333703, 0.3333333333333333703, 0.3333333333333333703, 0.3333333333333333703, 0.3333333333333333703, 0.3333333333333333703, 0.3333333333333333703, 0.3333333333333333703, 0.3333333333333333703, 0.3333333333333333703),
 ( 1.000000000000000000, 1.000000000000000000, 1.000000000000000000, 1.000000000000000000, 1.000000000000000000, 1.000000000000000000, 1.000000000000000000, 1.000000000000000000, 1.000000000000000000, 1.000000000000000000, 1.000000000000000000, 1.000000000000000000, 1.000000000000000000, 1.000000000000000000, 1.000000000000000000, 1.000000000000000000, 1.000000000000000000, 1.000000000000000000, 1.000000000000000000, 1.000000000000000000, 1.000000000000000000, 1.000000000000000000, 1.000000000000000000, 1.000000000000000000, 1.000000000000000000, 1.000000000000000000, 1.000000000000000000, 1.000000000000000000, 1.000000000000000000, 1.000000000000000000, 1.000000000000000000, 1.000000000000000000, 1.000000000000000000, 1.000000000000000000, 1.000000000000000000, 1.000000000000000000, 1.000000000000000000, 1.000000000000000000) ) ) 
 REPRESENTATION_ITEM ( '' )  SURFACE ( )  );
#1834 = EDGE_CURVE ( 'NONE', #1160, #2642, #4755, .T. ) ;
#1835 = FACE_OUTER_BOUND ( 'NONE', #4872, .T. ) ;
#1836 = CARTESIAN_POINT ( 'NONE',  ( 36.66581985038887126, 25.00000000000018474, 340.1662229844756098 ) ) ;
#1837 = SHAPE_DEFINITION_REPRESENTATION ( #2548, #2124 ) ;
#1838 = EDGE_CURVE ( 'NONE', #3404, #783, #3435, .T. ) ;
#1839 = EDGE_CURVE ( 'NONE', #4953, #1676, #2123, .T. ) ;
#1840 = ORIENTED_EDGE ( 'NONE', *, *, #1838, .T. ) ;
#1841 = CARTESIAN_POINT ( 'NONE',  ( 33.59898979596707136, 25.00000000000018474, 384.0431050523492900 ) ) ;
#1842 = ORIENTED_EDGE ( 'NONE', *, *, #1946, .F. ) ;
#1843 = CARTESIAN_POINT ( 'NONE',  ( -48.13570084519476211, 15.00000000000001421, 62.68703548022115513 ) ) ;
#1844 = PLANE ( 'NONE',  #3472 ) ;
#1845 = CIRCLE ( 'NONE', #4745, 4.382543221487789076 ) ;
#1846 = VERTEX_POINT ( 'NONE', #4637 ) ;
#1847 = EDGE_LOOP ( 'NONE', ( #769, #2593 ) ) ;
#1848 = DIRECTION ( 'NONE',  ( 0.01527226085271977431, 2.087708059715749652E-31, 0.9998833722232041143 ) ) ;
#1849 = CARTESIAN_POINT ( 'NONE',  ( 131.3198108831832656, 84.98551036222518462, -10.00000000000000888 ) ) ;
#1850 = LINE ( 'NONE', #1444, #4852 ) ;
#1851 = DIRECTION ( 'NONE',  ( 0.000000000000000000, -1.000000000000000000, 0.000000000000000000 ) ) ;
#1852 = ORIENTED_EDGE ( 'NONE', *, *, #4380, .T. ) ;
#1853 = EDGE_CURVE ( 'NONE', #5006, #1449, #191, .T. ) ;
#1854 = EDGE_CURVE ( 'NONE', #4228, #1349, #4156, .T. ) ;
#1855 = DIRECTION ( 'NONE',  ( 5.551115123125772841E-17, -1.848892746611743135E-31, -1.000000000000000000 ) ) ;
#1856 = CARTESIAN_POINT ( 'NONE',  ( -49.96441683051492078, -24.99999999999981881, 542.4422122871054626 ) ) ;
#1857 = DIRECTION ( 'NONE',  ( 1.000000000000000000, 0.000000000000000000, 0.000000000000000000 ) ) ;
#1858 = AXIS2_PLACEMENT_3D ( 'NONE', #1680, #4609, #844 ) ;
#1859 = CARTESIAN_POINT ( 'NONE',  ( 159.4907110033991273, 15.00000000000001421, 139.1303977902171596 ) ) ;
#1860 = VECTOR ( 'NONE', #1558, 1000.000000000000000 ) ;
#1861 = AXIS2_PLACEMENT_3D ( 'NONE', #2922, #3772, #4216 ) ;
#1862 = CARTESIAN_POINT ( 'NONE',  ( -349.7655555707380017, 2.222614453595284090E-15, 158.2793954369929850 ) ) ;
#1863 = CARTESIAN_POINT ( 'NONE',  ( -30.63277980166709114, 25.00000000000018474, 527.1358351633700750 ) ) ;
#1864 = ADVANCED_FACE ( 'NONE', ( #2079 ), #4253, .T. ) ;
#1865 = AXIS2_PLACEMENT_3D ( 'NONE', #4756, #2781, #1409 ) ;
#1866 = AXIS2_PLACEMENT_3D ( 'NONE', #2020, #4139, #4167 ) ;
#1867 = EDGE_LOOP ( 'NONE', ( #371, #2172 ) ) ;
#1868 = CARTESIAN_POINT ( 'NONE',  ( 16.26935751051938439, 25.00000000000000355, 140.3055424402287770 ) ) ;
#1869 = ORIENTED_EDGE ( 'NONE', *, *, #2944, .F. ) ;
#1870 = EDGE_CURVE ( 'NONE', #3390, #4488, #3186, .T. ) ;
#1871 = ADVANCED_FACE ( 'NONE', ( #489 ), #2902, .T. ) ;
#1872 = DIRECTION ( 'NONE',  ( 0.09383933793885568253, -2.673190762809473730E-31, -0.9955873536034882676 ) ) ;
#1873 = AXIS2_PLACEMENT_3D ( 'NONE', #3403, #804, #887 ) ;
#1874 = CARTESIAN_POINT ( 'NONE',  ( -347.8887688119603467, 2.222614453595284090E-15, 138.3676483649222178 ) ) ;
#1875 = CIRCLE ( 'NONE', #5025, 1.000000000000000888 ) ;
#1876 = EDGE_LOOP ( 'NONE', ( #2893, #3939 ) ) ;
#1877 = CIRCLE ( 'NONE', #1262, 6.000000000000032863 ) ;
#1878 = ORIENTED_EDGE ( 'NONE', *, *, #3507, .F. ) ;
#1879 = CARTESIAN_POINT ( 'NONE',  ( -365.8191009029663974, 5.636683259291067391E-15, 36.23439996194950652 ) ) ;
#1880 = CARTESIAN_POINT ( 'NONE',  ( -347.7949294740212736, 2.222614453595284090E-15, 137.3720610113191469 ) ) ;
#1881 = CARTESIAN_POINT ( 'NONE',  ( -82.68018911681710392, 75.92317977368848858, -9.999999999999953815 ) ) ;
#1882 = FACE_OUTER_BOUND ( 'NONE', #109, .T. ) ;
#1883 = CIRCLE ( 'NONE', #3815, 5.250000000000004441 ) ;
#1884 = CIRCLE ( 'NONE', #4955, 27.50000000000126832 ) ;
#1885 = CARTESIAN_POINT ( 'NONE',  ( 137.9714219172562366, 84.45434506795687923, -12.00000000000001066 ) ) ;
#1886 = ORIENTED_EDGE ( 'NONE', *, *, #728, .F. ) ;
#1887 = VECTOR ( 'NONE', #2790, 1000.000000000000000 ) ;
#1888 =( NAMED_UNIT ( * ) SI_UNIT ( $, .STERADIAN. ) SOLID_ANGLE_UNIT ( ) );
#1889 = DIRECTION ( 'NONE',  ( -5.679099018122554920E-31, -1.000000000000000000, 2.149753974990777610E-31 ) ) ;
#1890 = CARTESIAN_POINT ( 'NONE',  ( 5.624351423727398824, -24.99999999999981881, 474.0483466084681368 ) ) ;
#1891 = PLANE ( 'NONE',  #2761 ) ;
#1892 = CARTESIAN_POINT ( 'NONE',  ( 137.9714219172561513, 98.45434506795687923, -12.00000000000006573 ) ) ;
#1893 = CARTESIAN_POINT ( 'NONE',  ( -349.7655555707380017, 2.222614453595284090E-15, 158.2793954369929850 ) ) ;
#1894 = DIRECTION ( 'NONE',  ( -0.9998833722232040033, 6.797399803719615819E-31, 0.01527226085271964420 ) ) ;
#1895 = APPLICATION_PROTOCOL_DEFINITION ( 'draft international standard', 'automotive_design', 1998, #2438 ) ;
#1896 = CARTESIAN_POINT ( 'NONE',  ( -268.5984117390374877, 3.740497495074990297E-15, 475.6392848759629715 ) ) ;
#1897 = EDGE_LOOP ( 'NONE', ( #2430, #69, #5075, #5204 ) ) ;
#1898 = CARTESIAN_POINT ( 'NONE',  ( 11.65205807320734976, 3.740497495074990297E-15, 340.0738060255405912 ) ) ;
#1899 = EDGE_LOOP ( 'NONE', ( #3785, #3231, #671, #1543, #3257, #2235, #2137, #1668 ) ) ;
#1900 = CARTESIAN_POINT ( 'NONE',  ( -80.02857808274410445, -21.54565493204320248, -26.84924240491759662 ) ) ;
#1901 = FACE_OUTER_BOUND ( 'NONE', #3610, .T. ) ;
#1902 = EDGE_LOOP ( 'NONE', ( #583, #3455, #4112, #1482 ) ) ;
#1903 = VERTEX_POINT ( 'NONE', #3737 ) ;
#1904 = CARTESIAN_POINT ( 'NONE',  ( -321.4851553309757151, 5.712857831165392007E-15, 161.9494039218531043 ) ) ;
#1905 = FACE_BOUND ( 'NONE', #4578, .T. ) ;
#1906 = EDGE_CURVE ( 'NONE', #2162, #1002, #5040, .T. ) ;
#1907 = DIRECTION ( 'NONE',  ( 5.551115123125772841E-17, -1.848892746611743135E-31, -1.000000000000000000 ) ) ;
#1908 = CARTESIAN_POINT ( 'NONE',  ( -98.02857808274411866, 84.45434506795672291, 5.551115123125782702E-14 ) ) ;
#1909 = AXIS2_PLACEMENT_3D ( 'NONE', #1557, #5285, #4063 ) ;
#1910 = LINE ( 'NONE', #177, #204 ) ;
#1911 = ORIENTED_EDGE ( 'NONE', *, *, #4038, .F. ) ;
#1912 = AXIS2_PLACEMENT_3D ( 'NONE', #3579, #5237, #3166 ) ;
#1913 = DIRECTION ( 'NONE',  ( 0.9955873536034882676, -5.273458392682099492E-31, 0.09383933793885600172 ) ) ;
#1914 = CARTESIAN_POINT ( 'NONE',  ( -367.0460729392618191, -24.99999999999981881, 268.0688838304706678 ) ) ;
#1915 = DIRECTION ( 'NONE',  ( 0.01527226085271972227, 2.095411779493299033E-31, 0.9998833722232041143 ) ) ;
#1916 = CARTESIAN_POINT ( 'NONE',  ( -78.28422483266226095, 85.40608534173227895, -10.00000000000006395 ) ) ;
#1917 = EDGE_CURVE ( 'NONE', #4985, #3013, #2523, .T. ) ;
#1918 = DIRECTION ( 'NONE',  ( 0.9983803615885644689, 0.000000000000000000, 0.05689159511111529371 ) ) ;
#1919 = CARTESIAN_POINT ( 'NONE',  ( 12.58979647763672283, 2.222614453595284090E-15, 97.46177917736021357 ) ) ;
#1920 = PRODUCT_CONTEXT ( 'NONE', #256, 'mechanical' ) ;
#1921 = CARTESIAN_POINT ( 'NONE',  ( -48.20943979674346735, -24.99999999999981881, 509.2978244404901602 ) ) ;
#1922 = CARTESIAN_POINT ( 'NONE',  ( 24.85474708473287109, 3.252606517456513302E-16, 216.1905617304896623 ) ) ;
#1923 = ORIENTED_EDGE ( 'NONE', *, *, #1376, .F. ) ;
#1924 = CARTESIAN_POINT ( 'NONE',  ( -312.0566616799260373, 24.99999999999997158, 419.2731246273838792 ) ) ;
#1925 = ORIENTED_EDGE ( 'NONE', *, *, #1036, .T. ) ;
#1926 = CARTESIAN_POINT ( 'NONE',  ( 137.9714219172561798, -39.54565493204318471, -5.551115123125782702E-14 ) ) ;
#1927 = DIRECTION ( 'NONE',  ( 0.000000000000000000, 1.000000000000000000, 0.000000000000000000 ) ) ;
#1928 = ADVANCED_FACE ( 'NONE', ( #1636 ), #2958, .T. ) ;
#1929 = ORIENTED_EDGE ( 'NONE', *, *, #5256, .F. ) ;
#1930 = VERTEX_POINT ( 'NONE', #3351 ) ;
#1931 = CARTESIAN_POINT ( 'NONE',  ( -320.4162772499240077, -1.001483571081362644E-29, 139.9526428046378044 ) ) ;
#1932 = CARTESIAN_POINT ( 'NONE',  ( -338.5048350180761076, 2.276824562219559311E-15, 38.80891300457378890 ) ) ;
#1933 = CARTESIAN_POINT ( 'NONE',  ( -84.02857808274400497, -39.54565493204319893, -11.99999999999984368 ) ) ;
#1934 = CARTESIAN_POINT ( 'NONE',  ( 131.3198108831831519, -26.07682022631159668, -12.00000000000001066 ) ) ;
#1935 = EDGE_CURVE ( 'NONE', #3692, #2650, #455, .T. ) ;
#1936 = FILL_AREA_STYLE ('',( #642 ) ) ;
#1937 = VERTEX_POINT ( 'NONE', #2571 ) ;
#1938 = ADVANCED_FACE ( 'NONE', ( #3326 ), #4688, .T. ) ;
#1939 = ADVANCED_FACE ( 'NONE', ( #4178 ), #4235, .T. ) ;
#1940 = LINE ( 'NONE', #3574, #1370 ) ;
#1941 = DIRECTION ( 'NONE',  ( -5.551115123125772841E-17, 1.848892746611743135E-31, 1.000000000000000000 ) ) ;
#1942 = ADVANCED_FACE ( 'NONE', ( #1226 ), #408, .T. ) ;
#1943 = DIRECTION ( 'NONE',  ( 0.000000000000000000, 0.000000000000000000, -1.000000000000000000 ) ) ;
#1944 = DIRECTION ( 'NONE',  ( -0.9955873536034882676, 5.498529991225532962E-31, -0.09383933793885550212 ) ) ;
#1945 = DIRECTION ( 'NONE',  ( -0.4205749795070158337, -0.9072577839912276954, 0.000000000000000000 ) ) ;
#1946 = EDGE_CURVE ( 'NONE', #3835, #3650, #2100, .T. ) ;
#1947 = CARTESIAN_POINT ( 'NONE',  ( 151.9714219172563219, 84.45434506795677976, -5.551115123125782702E-14 ) ) ;
#1948 = CARTESIAN_POINT ( 'NONE',  ( -80.59222536594943165, 25.00000000000018474, 529.1597157429057461 ) ) ;
#1949 = CARTESIAN_POINT ( 'NONE',  ( 5.624351423727398824, -24.99999999999981881, 474.0483466084681368 ) ) ;
#1950 = DIRECTION ( 'NONE',  ( 0.4205749795070158337, 0.9072577839912276954, 0.000000000000000000 ) ) ;
#1951 = CIRCLE ( 'NONE', #3623, 28.50000000000127898 ) ;
#1952 = ORIENTED_EDGE ( 'NONE', *, *, #2647, .T. ) ;
#1953 = CARTESIAN_POINT ( 'NONE',  ( -156.9923520473274721, 25.00000000000018474, 556.8176423728723421 ) ) ;
#1954 = ORIENTED_EDGE ( 'NONE', *, *, #2417, .F. ) ;
#1955 = AXIS2_PLACEMENT_3D ( 'NONE', #2434, #4959, #3677 ) ;
#1956 = CARTESIAN_POINT ( 'NONE',  ( -0.6802310551622114954, 2.222614453595284090E-15, 47.14310755735262859 ) ) ;
#1957 = DIRECTION ( 'NONE',  ( -0.05689159511111523820, 0.000000000000000000, 0.9983803615885644689 ) ) ;
#1958 = AXIS2_PLACEMENT_3D ( 'NONE', #5052, #4242, #1296 ) ;
#1959 = EDGE_CURVE ( 'NONE', #744, #3745, #1069, .T. ) ;
#1960 = TOROIDAL_SURFACE ( 'NONE', #2662, 30.50000000000110845, 1.000000000000000000 ) ;
#1961 = ORIENTED_EDGE ( 'NONE', *, *, #2485, .F. ) ;
#1962 = VECTOR ( 'NONE', #4882, 999.9999999999998863 ) ;
#1963 =( GEOMETRIC_REPRESENTATION_CONTEXT ( 3 ) GLOBAL_UNCERTAINTY_ASSIGNED_CONTEXT ( ( #775 ) ) GLOBAL_UNIT_ASSIGNED_CONTEXT ( ( #2148, #4210, #4671 ) ) REPRESENTATION_CONTEXT ( 'NONE', 'WORKASPACE' ) );
#1964 = ORIENTED_EDGE ( 'NONE', *, *, #1376, .T. ) ;
#1965 = CARTESIAN_POINT ( 'NONE',  ( -351.6423423295148041, 5.421010862427522170E-17, 178.1911425090623311 ) ) ;
#1966 = CARTESIAN_POINT ( 'NONE',  ( 29.23877717791895492, 0.000000000000000000, 67.09613410133256650 ) ) ;
#1967 = DIRECTION ( 'NONE',  ( 0.000000000000000000, 1.000000000000000000, 0.000000000000000000 ) ) ;
#1968 = DIRECTION ( 'NONE',  ( 1.000000000000000000, 0.000000000000000000, 0.000000000000000000 ) ) ;
#1969 = TOROIDAL_SURFACE ( 'NONE', #3728, 28.50000000000115818, 1.000000000000000000 ) ;
#1970 = CARTESIAN_POINT ( 'NONE',  ( -338.5986743560152377, -14.95948628165117178, 39.80450035817695209 ) ) ;
#1971 = ORIENTED_EDGE ( 'NONE', *, *, #275, .T. ) ;
#1972 = EDGE_CURVE ( 'NONE', #4236, #4708, #4929, .T. ) ;
#1973 = FACE_OUTER_BOUND ( 'NONE', #1286, .T. ) ;
#1974 = AXIS2_PLACEMENT_3D ( 'NONE', #3415, #872, #3845 ) ;
#1975 = DIRECTION ( 'NONE',  ( 0.000000000000000000, 1.000000000000000000, 0.000000000000000000 ) ) ;
#1976 = CARTESIAN_POINT ( 'NONE',  ( -322.4807426845795817, 2.222614453595269496E-15, 161.8555645839142016 ) ) ;
#1977 = VECTOR ( 'NONE', #10, 999.9999999999998863 ) ;
#1978 = CARTESIAN_POINT ( 'NONE',  ( 29.23877717791900466, 15.00000000000001421, 117.0961341013326233 ) ) ;
#1979 = VECTOR ( 'NONE', #5235, 1000.000000000000000 ) ;
#1980 = CARTESIAN_POINT ( 'NONE',  ( 131.3198108831832087, -26.07682022631159668, -10.00000000000000888 ) ) ;
#1981 = CARTESIAN_POINT ( 'NONE',  ( 11.65205807320727871, 25.00000000000018474, 340.0738060255407049 ) ) ;
#1982 = CARTESIAN_POINT ( 'NONE',  ( -14.89480152442222582, -24.99999999999981881, 508.6517828409982940 ) ) ;
#1983 = LINE ( 'NONE', #2801, #3462 ) ;
#1984 = VERTEX_POINT ( 'NONE', #3891 ) ;
#1985 = CARTESIAN_POINT ( 'NONE',  ( -13.17877320795268759, 1.897353801849632760E-15, 47.33401081801291355 ) ) ;
#1986 = ORIENTED_EDGE ( 'NONE', *, *, #792, .F. ) ;
#1987 = FACE_OUTER_BOUND ( 'NONE', #3292, .T. ) ;
#1988 = DIRECTION ( 'NONE',  ( 0.000000000000000000, 1.000000000000000000, 0.000000000000000000 ) ) ;
#1989 = ORIENTED_EDGE ( 'NONE', *, *, #3060, .T. ) ;
#1990 = PRODUCT_DEFINITION_CONTEXT ( 'detailed design', #2817, 'design' ) ;
#1991 = ORIENTED_EDGE ( 'NONE', *, *, #2250, .F. ) ;
#1992 = CYLINDRICAL_SURFACE ( 'NONE', #4938, 22.67218956682437536 ) ;
#1993 = DIRECTION ( 'NONE',  ( -0.9955873536034881566, 5.462637660443544243E-31, -0.09383933793885600172 ) ) ;
#1994 = DIRECTION ( 'NONE',  ( 0.9072577839912275843, 0.4205749795070160002, 1.110223024625155801E-16 ) ) ;
#1995 = CARTESIAN_POINT ( 'NONE',  ( -340.0535087002904220, 14.95948628165116823, 101.9421712359864500 ) ) ;
#1996 = LINE ( 'NONE', #3396, #3113 ) ;
#1997 = EDGE_LOOP ( 'NONE', ( #4025, #2747, #1259, #4606 ) ) ;
#1998 = DIRECTION ( 'NONE',  ( -0.9998833722232040033, 6.797399803719615819E-31, 0.01527226085271964420 ) ) ;
#1999 = DIRECTION ( 'NONE',  ( -0.9955873536034882676, 5.502656983963329947E-31, -0.09383933793885568253 ) ) ;
#2000 = CARTESIAN_POINT ( 'NONE',  ( -338.5048350180761076, 2.276824562219559311E-15, 38.80891300457378890 ) ) ;
#2001 = CARTESIAN_POINT ( 'NONE',  ( -351.6423423295148041, 5.421010862427522170E-17, 178.1911425090623311 ) ) ;
#2002 = SURFACE_STYLE_USAGE ( .BOTH. , #2472 ) ;
#2003 = VECTOR ( 'NONE', #3266, 1000.000000000000000 ) ;
#2004 = DIRECTION ( 'NONE',  ( 1.000000000000000000, -5.720779902258398713E-31, 0.000000000000000000 ) ) ;
#2005 = CARTESIAN_POINT ( 'NONE',  ( -36.58361131987999926, 25.00000000000018474, 532.6725316595209279 ) ) ;
#2006 = CONTEXT_DEPENDENT_SHAPE_REPRESENTATION ( #2154, #5302 ) ;
#2007 = CARTESIAN_POINT ( 'NONE',  ( -354.3266237013165778, -24.99999999999981881, 381.2801272015587983 ) ) ;
#2008 = EDGE_CURVE ( 'NONE', #1438, #4669, #1421, .T. ) ;
#2009 = ORIENTED_EDGE ( 'NONE', *, *, #1959, .T. ) ;
#2010 = CARTESIAN_POINT ( 'NONE',  ( 11.35554381053716000, 3.794707603699265519E-15, 353.5846600851142512 ) ) ;
#2011 = ORIENTED_EDGE ( 'NONE', *, *, #2435, .F. ) ;
#2012 = ADVANCED_FACE ( 'NONE', ( #95 ), #5099, .F. ) ;
#2013 = EDGE_CURVE ( 'NONE', #1574, #744, #4837, .T. ) ;
#2014 = DIRECTION ( 'NONE',  ( -0.9955873536034882676, 5.452307672560241053E-31, -0.09383933793885547436 ) ) ;
#2015 = EDGE_CURVE ( 'NONE', #3533, #496, #122, .T. ) ;
#2016 = DIRECTION ( 'NONE',  ( 0.09383933793885568253, -2.673190762809473730E-31, -0.9955873536034882676 ) ) ;
#2017 = ORIENTED_EDGE ( 'NONE', *, *, #414, .F. ) ;
#2018 = ORIENTED_EDGE ( 'NONE', *, *, #5259, .F. ) ;
#2019 = PRODUCT_DEFINITION_SHAPE ( 'NONE', 'NONE',  #4505 ) ;
#2020 = CARTESIAN_POINT ( 'NONE',  ( 133.9714219172562366, -21.54565493204319182, -12.00000000000006573 ) ) ;
#2021 = DIRECTION ( 'NONE',  ( -1.000000000000000000, 3.759415251443877379E-31, -5.551115123125772841E-17 ) ) ;
#2022 = CARTESIAN_POINT ( 'NONE',  ( 119.2387771779189478, -14.99999999999998579, 167.0961341013325523 ) ) ;
#2023 = DIRECTION ( 'NONE',  ( -0.9955873536034882676, 5.273458392682099492E-31, -0.09383933793885600172 ) ) ;
#2024 = DIRECTION ( 'NONE',  ( -0.9955873536034882676, 5.273458392682099492E-31, -0.09383933793885600172 ) ) ;
#2025 = ORIENTED_EDGE ( 'NONE', *, *, #4925, .T. ) ;
#2026 = ORIENTED_EDGE ( 'NONE', *, *, #1959, .F. ) ;
#2027 = LINE ( 'NONE', #3682, #821 ) ;
#2028 = CARTESIAN_POINT ( 'NONE',  ( -80.60298687151650654, 2.222614453595284090E-15, 555.2885198911399129 ) ) ;
#2029 = CARTESIAN_POINT ( 'NONE',  ( 102.9433289385998478, 15.00000000000001421, 135.9081080810072137 ) ) ;
#2030 = ADVANCED_FACE ( 'NONE', ( #3492 ), #2733, .T. ) ;
#2031 = EDGE_CURVE ( 'NONE', #3095, #4078, #1767, .T. ) ;
#2032 = CARTESIAN_POINT ( 'NONE',  ( -353.5191290882918338, 0.000000000000000000, 198.1028895811323025 ) ) ;
#2033 = DIRECTION ( 'NONE',  ( 0.09383933793885568253, -2.673190762809473730E-31, -0.9955873536034882676 ) ) ;
#2034 = CARTESIAN_POINT ( 'NONE',  ( 11.35554381052501682, 25.00000000000018474, 353.5846600851141943 ) ) ;
#2035 = CARTESIAN_POINT ( 'NONE',  ( 36.35777514575907787, -24.99999999999981881, 354.7349908125917750 ) ) ;
#2036 = ORIENTED_EDGE ( 'NONE', *, *, #1230, .T. ) ;
#2037 = ORIENTED_EDGE ( 'NONE', *, *, #499, .F. ) ;
#2038 = DIRECTION ( 'NONE',  ( -0.9955873536034882676, 5.498529991225532086E-31, -0.09383933793885536334 ) ) ;
#2039 = DIRECTION ( 'NONE',  ( -0.9955873536034882676, 5.456801509096968857E-31, -0.09383933793885568253 ) ) ;
#2040 = AXIS2_PLACEMENT_3D ( 'NONE', #451, #3378, #892 ) ;
#2041 = VERTEX_POINT ( 'NONE', #1825 ) ;
#2042 = EDGE_CURVE ( 'NONE', #1788, #3474, #1366, .T. ) ;
#2043 = VECTOR ( 'NONE', #5278, 1000.000000000000000 ) ;
#2044 = DIRECTION ( 'NONE',  ( -1.219242865862094703E-16, 1.000000000000000000, -1.149200448409285278E-17 ) ) ;
#2045 = DIRECTION ( 'NONE',  ( 5.551115123125772841E-17, -1.848892746611743135E-31, -1.000000000000000000 ) ) ;
#2046 = CYLINDRICAL_SURFACE ( 'NONE', #3810, 31.50000000000125766 ) ;
#2047 = ORIENTED_EDGE ( 'NONE', *, *, #1906, .T. ) ;
#2048 = VECTOR ( 'NONE', #4447, 1000.000000000000000 ) ;
#2049 = AXIS2_PLACEMENT_3D ( 'NONE', #2724, #4405, #637 ) ;
#2050 = ORIENTED_EDGE ( 'NONE', *, *, #2176, .F. ) ;
#2051 = DIRECTION ( 'NONE',  ( 0.000000000000000000, 0.000000000000000000, -1.000000000000000000 ) ) ;
#2052 = DIRECTION ( 'NONE',  ( 0.01527226085271972227, 2.095411779493299033E-31, 0.9998833722232041143 ) ) ;
#2053 = AXIS2_PLACEMENT_3D ( 'NONE', #5343, #2378, #3216 ) ;
#2054 = COLOUR_RGB ( '',0.7921568627450980005, 0.8196078431372548767, 0.9333333333333333481 ) ;
#2055 = CARTESIAN_POINT ( 'NONE',  ( -80.02857808274418971, -21.54565493204321669, -2.000000000000001776 ) ) ;
#2056 = CIRCLE ( 'NONE', #3380, 14.00000000000002665 ) ;
#2057 = VECTOR ( 'NONE', #1293, 1000.000000000000000 ) ;
#2058 = CIRCLE ( 'NONE', #126, 14.00000000000002665 ) ;
#2059 = CARTESIAN_POINT ( 'NONE',  ( 8.821273309647297722, 3.740497495074990297E-15, 380.5076279642372015 ) ) ;
#2060 = CARTESIAN_POINT ( 'NONE',  ( -63.04765821498167355, 25.00000000000018474, 521.0401840782875524 ) ) ;
#2061 = CARTESIAN_POINT ( 'NONE',  ( -80.60298687151650654, 2.222614453595284090E-15, 555.2885198911399129 ) ) ;
#2062 = AXIS2_PLACEMENT_3D ( 'NONE', #1038, #3135, #2690 ) ;
#2063 = AXIS2_PLACEMENT_3D ( 'NONE', #4028, #5340, #3214 ) ;
#2064 = PRODUCT_DEFINITION_SHAPE ( 'NONE', 'NONE',  #5408 ) ;
#2065 = EDGE_LOOP ( 'NONE', ( #4076, #3044, #2483, #1693, #2979, #3093, #1816, #2995 ) ) ;
#2066 = EDGE_CURVE ( 'NONE', #4617, #5050, #2911, .T. ) ;
#2067 = DIRECTION ( 'NONE',  ( -0.9955873536034882676, 5.436595176548168253E-31, -0.09383933793885573804 ) ) ;
#2068 = ORIENTED_EDGE ( 'NONE', *, *, #3416, .F. ) ;
#2069 = ORIENTED_EDGE ( 'NONE', *, *, #5256, .T. ) ;
#2070 = DIRECTION ( 'NONE',  ( -0.9955873536034886007, 6.162975822039140717E-31, -0.09383933793885225472 ) ) ;
#2071 = CARTESIAN_POINT ( 'NONE',  ( -329.5232379498077080, 5.421010862427522170E-17, 102.9347045701690604 ) ) ;
#2072 = DIRECTION ( 'NONE',  ( 0.000000000000000000, -1.000000000000000000, 0.000000000000000000 ) ) ;
#2073 = DIRECTION ( 'NONE',  ( -0.9072577839912275843, -0.4205749795070160002, -1.110223024625155801E-16 ) ) ;
#2074 = ORIENTED_EDGE ( 'NONE', *, *, #1839, .T. ) ;
#2075 = EDGE_CURVE ( 'NONE', #3556, #2890, #1673, .T. ) ;
#2076 = ORIENTED_EDGE ( 'NONE', *, *, #2008, .T. ) ;
#2077 = CARTESIAN_POINT ( 'NONE',  ( 0.000000000000000000, 80.00000000000000000, 0.000000000000000000 ) ) ;
#2078 = EDGE_CURVE ( 'NONE', #3069, #3692, #4743, .T. ) ;
#2079 = FACE_OUTER_BOUND ( 'NONE', #2065, .T. ) ;
#2080 = CARTESIAN_POINT ( 'NONE',  ( -353.5191290882918338, 0.000000000000000000, 198.1028895811323025 ) ) ;
#2081 = VECTOR ( 'NONE', #620, 1000.000000000000114 ) ;
#2082 = CYLINDRICAL_SURFACE ( 'NONE', #3291, 12.50000000000003197 ) ;
#2083 = CARTESIAN_POINT ( 'NONE',  ( -39.32426838448843398, 3.740497495074990297E-15, 499.4571537926191240 ) ) ;
#2084 = CARTESIAN_POINT ( 'NONE',  ( -339.2542556961722084, 3.740497495074990297E-15, 239.6247169981598972 ) ) ;
#2085 = DIRECTION ( 'NONE',  ( -5.551115123125772841E-17, 1.848892746611743135E-31, 1.000000000000000000 ) ) ;
#2086 = AXIS2_PLACEMENT_3D ( 'NONE', #2292, #5154, #2635 ) ;
#2087 = VERTEX_POINT ( 'NONE', #5229 ) ;
#2088 = VECTOR ( 'NONE', #2203, 1000.000000000000114 ) ;
#2089 = CIRCLE ( 'NONE', #1821, 12.50000000000009237 ) ;
#2090 = DIRECTION ( 'NONE',  ( 0.09383933793885568253, -2.673190762809473730E-31, -0.9955873536034882676 ) ) ;
#2091 = CARTESIAN_POINT ( 'NONE',  ( 133.9714219172562366, -21.54565493204323090, -9.999999999999841904 ) ) ;
#2092 = AXIS2_PLACEMENT_3D ( 'NONE', #4125, #5263, #2359 ) ;
#2093 = EDGE_LOOP ( 'NONE', ( #2281, #3488, #4945 ) ) ;
#2094 = CARTESIAN_POINT ( 'NONE',  ( 131.3198108831831519, -26.07682022631159668, -12.00000000000001066 ) ) ;
#2095 = CARTESIAN_POINT ( 'NONE',  ( -342.9618789639491752, -14.95948628165117178, 39.39324540378412109 ) ) ;
#2096 = CARTESIAN_POINT ( 'NONE',  ( -380.0371305177060322, 3.252606517456679456E-16, 154.4217082762537245 ) ) ;
#2097 = ORIENTED_EDGE ( 'NONE', *, *, #695, .T. ) ;
#2098 = ORIENTED_EDGE ( 'NONE', *, *, #4790, .F. ) ;
#2099 = DIRECTION ( 'NONE',  ( -0.01527226085271972227, -2.080004339938201146E-31, -0.9998833722232041143 ) ) ;
#2100 = LINE ( 'NONE', #2193, #5272 ) ;
#2101 = CARTESIAN_POINT ( 'NONE',  ( -108.3530091724271358, 15.00000000000001421, 123.8676211295743599 ) ) ;
#2102 = EDGE_CURVE ( 'NONE', #2695, #4403, #1951, .T. ) ;
#2103 = EDGE_CURVE ( 'NONE', #5397, #4871, #3453, .T. ) ;
#2104 = DIRECTION ( 'NONE',  ( 0.9955873536034883786, -5.498529991225525955E-31, 0.09383933793885444741 ) ) ;
#2105 = EDGE_CURVE ( 'NONE', #850, #3157, #3152, .T. ) ;
#2106 = ADVANCED_FACE ( 'NONE', ( #3947 ), #3538, .T. ) ;
#2107 = CARTESIAN_POINT ( 'NONE',  ( -349.6717162327985307, 3.252606517456513302E-16, 157.2838080833889194 ) ) ;
#2108 = CARTESIAN_POINT ( 'NONE',  ( -23.53079058812296154, 3.740497495074990297E-15, 476.4235034963361954 ) ) ;
#2109 = PLANE ( 'NONE',  #914 ) ;
#2110 = ADVANCED_FACE ( 'NONE', ( #3129, #4794 ), #3969, .T. ) ;
#2111 = VERTEX_POINT ( 'NONE', #5251 ) ;
#2112 = ORIENTED_EDGE ( 'NONE', *, *, #1834, .T. ) ;
#2113 = CARTESIAN_POINT ( 'NONE',  ( -338.5048350180761076, 2.276824562219559311E-15, 38.80891300457378890 ) ) ;
#2114 = SHAPE_REPRESENTATION_RELATIONSHIP ( 'NONE' , 'NONE' ,  #3079, #4432 ) ;
#2115 = SURFACE_STYLE_FILL_AREA ( #2533 ) ;
#2116 = VERTEX_POINT ( 'NONE', #3653 ) ;
#2117 = DIRECTION ( 'NONE',  ( 5.551115123125772841E-17, -1.848892746611743135E-31, -1.000000000000000000 ) ) ;
#2118 = CARTESIAN_POINT ( 'NONE',  ( -381.0327178713096714, 6.080251870909624272E-15, 154.3278689383148503 ) ) ;
#2119 = DIRECTION ( 'NONE',  ( -0.09383933793885568253, 2.673190762809473730E-31, 0.9955873536034882676 ) ) ;
#2120 = CARTESIAN_POINT ( 'NONE',  ( -376.4176382211731493, 1.317201266864838728E-29, 195.9445848085386217 ) ) ;
#2121 = CYLINDRICAL_SURFACE ( 'NONE', #1163, 17.00000000000009948 ) ;
#2122 = CARTESIAN_POINT ( 'NONE',  ( -74.02857808274417550, -21.54565493204321669, -2.000000000000001332 ) ) ;
#2123 = CIRCLE ( 'NONE', #711, 6.000000000000032863 ) ;
#2124 = SHAPE_REPRESENTATION ( 'MAT-023', ( #3309, #840, #2770, #2597, #2156, #220 ), #5396 ) ;
#2125 = ORIENTED_EDGE ( 'NONE', *, *, #1436, .T. ) ;
#2126 = VERTEX_POINT ( 'NONE', #4839 ) ;
#2127 = AXIS2_PLACEMENT_3D ( 'NONE', #1630, #1220, #479 ) ;
#2128 = EDGE_LOOP ( 'NONE', ( #4087, #1822, #5213, #1464 ) ) ;
#2129 = CARTESIAN_POINT ( 'NONE',  ( -347.7949294740212736, 2.222614453595284090E-15, 137.3720610113191469 ) ) ;
#2130 = DIRECTION ( 'NONE',  ( 5.551115123125772841E-17, -1.848892746611743135E-31, -1.000000000000000000 ) ) ;
#2131 = CARTESIAN_POINT ( 'NONE',  ( -342.9618789639491752, 14.95948628165116823, 39.39324540378412109 ) ) ;
#2132 = AXIS2_PLACEMENT_3D ( 'NONE', #1843, #4431, #4378 ) ;
#2133 = VECTOR ( 'NONE', #1517, 1000.000000000000114 ) ;
#2134 = ADVANCED_FACE ( 'NONE', ( #1602 ), #4523, .F. ) ;
#2135 = CARTESIAN_POINT ( 'NONE',  ( -98.02857808274411866, 84.45434506795672291, 5.551115123125782702E-14 ) ) ;
#2136 = AXIS2_PLACEMENT_3D ( 'NONE', #4511, #2868, #4188 ) ;
#2137 = ORIENTED_EDGE ( 'NONE', *, *, #3687, .T. ) ;
#2138 = AXIS2_PLACEMENT_3D ( 'NONE', #1554, #5252, #4469 ) ;
#2139 = CARTESIAN_POINT ( 'NONE',  ( -23.53079058812296154, 3.740497495074990297E-15, 476.4235034963361954 ) ) ;
#2140 = AXIS2_PLACEMENT_3D ( 'NONE', #951, #2220, #3896 ) ;
#2141 = CARTESIAN_POINT ( 'NONE',  ( -107.0991749147294172, 1.572093150103981429E-15, 535.0680222229615310 ) ) ;
#2142 = CARTESIAN_POINT ( 'NONE',  ( 137.9714219172560945, -39.54565493204318471, -11.99999999999995559 ) ) ;
#2143 = AXIS2_PLACEMENT_3D ( 'NONE', #1236, #2016, #4647 ) ;
#2144 = AXIS2_PLACEMENT_3D ( 'NONE', #3765, #1687, #412 ) ;
#2145 = EDGE_LOOP ( 'NONE', ( #4835, #1840, #1800, #5117 ) ) ;
#2146 = EDGE_LOOP ( 'NONE', ( #2036, #1964, #3011, #3872 ) ) ;
#2147 = CARTESIAN_POINT ( 'NONE',  ( -84.02857808274403340, 98.45434506795682239, -5.551115123125782702E-14 ) ) ;
#2148 =( LENGTH_UNIT ( ) NAMED_UNIT ( * ) SI_UNIT ( .MILLI., .METRE. ) );
#2149 = VECTOR ( 'NONE', #2547, 1000.000000000000000 ) ;
#2150 = DIRECTION ( 'NONE',  ( 0.09383933793885568253, -2.673190762809473730E-31, -0.9955873536034882676 ) ) ;
#2151 = VERTEX_POINT ( 'NONE', #3595 ) ;
#2152 = CYLINDRICAL_SURFACE ( 'NONE', #3811, 22.67218956682437536 ) ;
#2153 = AXIS2_PLACEMENT_3D ( 'NONE', #1708, #2073, #1222 ) ;
#2154 =( REPRESENTATION_RELATIONSHIP ('NONE','NONE', #2124, #4024 ) REPRESENTATION_RELATIONSHIP_WITH_TRANSFORMATION ( #4450 )SHAPE_REPRESENTATION_RELATIONSHIP( ) );
#2155 = DIRECTION ( 'NONE',  ( -0.9955873536034882676, 5.456801509096969733E-31, -0.09383933793885547436 ) ) ;
#2156 = AXIS2_PLACEMENT_3D ( 'NONE', #3908, #138, #3582 ) ;
#2157 = CARTESIAN_POINT ( 'NONE',  ( 0.07030049708446614587, -25.00000000000000355, 219.5055207296742026 ) ) ;
#2158 = CARTESIAN_POINT ( 'NONE',  ( 128.7214219172562366, -21.54565493204319182, -12.00000000000006573 ) ) ;
#2159 = DIRECTION ( 'NONE',  ( 0.09383933793885537722, -2.626968444144180508E-31, -0.9955873536034883786 ) ) ;
#2160 = PRODUCT_DEFINITION ( 'UNKNOWN', '', #404, #1990 ) ;
#2161 = ORIENTED_EDGE ( 'NONE', *, *, #795, .T. ) ;
#2162 = VERTEX_POINT ( 'NONE', #2759 ) ;
#2163 =( GEOMETRIC_REPRESENTATION_CONTEXT ( 3 ) GLOBAL_UNCERTAINTY_ASSIGNED_CONTEXT ( ( #4463 ) ) GLOBAL_UNIT_ASSIGNED_CONTEXT ( ( #2821, #2353, #4472 ) ) REPRESENTATION_CONTEXT ( 'NONE', 'WORKASPACE' ) );
#2164 = ORIENTED_EDGE ( 'NONE', *, *, #4862, .T. ) ;
#2165 = CARTESIAN_POINT ( 'NONE',  ( -365.8870837615305618, 2.625968386833868739E-15, 105.5338143064982717 ) ) ;
#2166 = DIRECTION ( 'NONE',  ( 0.000000000000000000, 0.000000000000000000, 1.000000000000000000 ) ) ;
#2167 = DIRECTION ( 'NONE',  ( 1.000000000000000000, -3.759415251443877379E-31, 5.551115123125772841E-17 ) ) ;
#2168 = ORIENTED_EDGE ( 'NONE', *, *, #2512, .F. ) ;
#2169 = CARTESIAN_POINT ( 'NONE',  ( -121.8424039466566313, 3.794707603699265519E-15, 535.4314447305365547 ) ) ;
#2170 = CARTESIAN_POINT ( 'NONE',  ( -16.96312831416352296, 1.572093150103981429E-15, 463.2830513152439380 ) ) ;
#2171 = CARTESIAN_POINT ( 'NONE',  ( 102.9433289385998478, 15.00000000000001421, 135.9081080810072137 ) ) ;
#2172 = ORIENTED_EDGE ( 'NONE', *, *, #1689, .F. ) ;
#2173 = ORIENTED_EDGE ( 'NONE', *, *, #2386, .F. ) ;
#2174 = DIRECTION ( 'NONE',  ( 0.09383933793885568253, -2.673190762809473730E-31, -0.9955873536034882676 ) ) ;
#2175 = EDGE_CURVE ( 'NONE', #742, #3068, #459, .T. ) ;
#2176 = EDGE_CURVE ( 'NONE', #5368, #483, #4412, .T. ) ;
#2177 = EDGE_CURVE ( 'NONE', #3314, #2087, #378, .T. ) ;
#2178 = ORIENTED_EDGE ( 'NONE', *, *, #1498, .F. ) ;
#2179 = CARTESIAN_POINT ( 'NONE',  ( 11.81831109762787690, 2.222614453595284090E-15, 46.95220429669389262 ) ) ;
#2180 = ADVANCED_FACE ( 'NONE', ( #4439 ), #639, .T. ) ;
#2181 = CIRCLE ( 'NONE', #5241, 1.000000000000000888 ) ;
#2182 = EDGE_CURVE ( 'NONE', #496, #2670, #4005, .T. ) ;
#2183 = CARTESIAN_POINT ( 'NONE',  ( 102.9433289385998478, 0.000000000000000000, 135.9081080810072137 ) ) ;
#2184 = CARTESIAN_POINT ( 'NONE',  ( -80.59222536594906217, 3.740497495074990297E-15, 529.1597157429033587 ) ) ;
#2185 = CARTESIAN_POINT ( 'NONE',  ( -367.0460729392618759, 0.000000000000000000, 268.0688838304710089 ) ) ;
#2186 = DIRECTION ( 'NONE',  ( 5.551115123125772841E-17, -1.848892746611743135E-31, -1.000000000000000000 ) ) ;
#2187 = AXIS2_PLACEMENT_3D ( 'NONE', #3251, #1499, #4069 ) ;
#2188 = ADVANCED_FACE ( 'NONE', ( #2348 ), #287, .F. ) ;
#2189 = ORIENTED_EDGE ( 'NONE', *, *, #4096, .T. ) ;
#2190 = ORIENTED_EDGE ( 'NONE', *, *, #4064, .F. ) ;
#2191 = ORIENTED_EDGE ( 'NONE', *, *, #2175, .F. ) ;
#2192 = LINE ( 'NONE', #94, #2416 ) ;
#2193 = CARTESIAN_POINT ( 'NONE',  ( -349.1289451064980085, 2.222614453595281723E-15, 38.81196702399444121 ) ) ;
#2194 = CARTESIAN_POINT ( 'NONE',  ( 127.9714219172561940, -21.54565493204319182, -2.000000000000002220 ) ) ;
#2195 = VERTEX_POINT ( 'NONE', #2377 ) ;
#2196 = CARTESIAN_POINT ( 'NONE',  ( -98.02857808274411866, 84.45434506795672291, 152.0000000000001990 ) ) ;
#2197 = CARTESIAN_POINT ( 'NONE',  ( -39.32426838448843398, 3.740497495074990297E-15, 499.4571537926191240 ) ) ;
#2198 = CARTESIAN_POINT ( 'NONE',  ( -312.7741936558949760, 5.421010862425789758E-17, 101.5000933658572677 ) ) ;
#2199 = EDGE_CURVE ( 'NONE', #5060, #3984, #545, .T. ) ;
#2200 = EDGE_CURVE ( 'NONE', #3237, #4329, #5342, .T. ) ;
#2201 = ORIENTED_EDGE ( 'NONE', *, *, #3959, .T. ) ;
#2202 = EDGE_LOOP ( 'NONE', ( #4249, #118 ) ) ;
#2203 = DIRECTION ( 'NONE',  ( 0.4205749795070158337, 0.9072577839912276954, 0.000000000000000000 ) ) ;
#2204 = ADVANCED_BREP_SHAPE_REPRESENTATION ( '', ( #4927, #4977, #1285, #3136, #2926 ), #5309 ) ;
#2205 = ORIENTED_EDGE ( 'NONE', *, *, #4780, .F. ) ;
#2206 = CARTESIAN_POINT ( 'NONE',  ( 31.14585677005082687, 2.222614453595284090E-15, 398.7793066466531968 ) ) ;
#2207 = EDGE_CURVE ( 'NONE', #4277, #2126, #1422, .T. ) ;
#2208 = EDGE_CURVE ( 'NONE', #2943, #3490, #2222, .T. ) ;
#2209 = CARTESIAN_POINT ( 'NONE',  ( -349.6717162327985307, 3.252606517456513302E-16, 157.2838080833889194 ) ) ;
#2210 = CARTESIAN_POINT ( 'NONE',  ( -339.2542556961734590, -24.99999999999981881, 239.6247169981589309 ) ) ;
#2211 = CARTESIAN_POINT ( 'NONE',  ( -354.3266237013149862, 5.421010862427522170E-17, 381.2801272015580025 ) ) ;
#2212 = CARTESIAN_POINT ( 'NONE',  ( -324.1698507674790335, 2.222614453595274229E-15, 179.7761369487778609 ) ) ;
#2213 = ORIENTED_EDGE ( 'NONE', *, *, #5430, .F. ) ;
#2214 = EDGE_LOOP ( 'NONE', ( #1852, #3085, #952, #4266 ) ) ;
#2215 = ORIENTED_EDGE ( 'NONE', *, *, #2177, .T. ) ;
#2216 = VECTOR ( 'NONE', #2607, 1000.000000000000000 ) ;
#2217 = DIRECTION ( 'NONE',  ( -0.9955873536034882676, 5.452307672560245432E-31, -0.09383933793885568253 ) ) ;
#2218 = DIRECTION ( 'NONE',  ( -1.000000000000000000, 0.000000000000000000, 0.000000000000000000 ) ) ;
#2219 = LINE ( 'NONE', #2194, #4166 ) ;
#2220 = DIRECTION ( 'NONE',  ( 0.09383933793885537722, -2.626968444144180508E-31, -0.9955873536034883786 ) ) ;
#2221 = ORIENTED_EDGE ( 'NONE', *, *, #3615, .F. ) ;
#2222 = CIRCLE ( 'NONE', #903, 4.382543221487789076 ) ;
#2223 = CYLINDRICAL_SURFACE ( 'NONE', #1817, 12.50000000000009237 ) ;
#2224 = CARTESIAN_POINT ( 'NONE',  ( 29.77542608467492613, 2.222614453595284090E-15, 249.2409987768030533 ) ) ;
#2225 = DIRECTION ( 'NONE',  ( -0.9955873536034882676, 5.436595176548168253E-31, -0.09383933793885573804 ) ) ;
#2226 = VECTOR ( 'NONE', #3228, 1000.000000000000000 ) ;
#2227 =( GEOMETRIC_REPRESENTATION_CONTEXT ( 3 ) GLOBAL_UNCERTAINTY_ASSIGNED_CONTEXT ( ( #282 ) ) GLOBAL_UNIT_ASSIGNED_CONTEXT ( ( #1628, #3850, #877 ) ) REPRESENTATION_CONTEXT ( 'NONE', 'WORKASPACE' ) );
#2228 = VERTEX_POINT ( 'NONE', #1577 ) ;
#2229 = CARTESIAN_POINT ( 'NONE',  ( 11.81831109762787690, 2.222614453595284090E-15, 46.95220429669389262 ) ) ;
#2230 = SHAPE_DEFINITION_REPRESENTATION ( #311, #3079 ) ;
#2231 = VECTOR ( 'NONE', #254, 1000.000000000000000 ) ;
#2232 = ORIENTED_EDGE ( 'NONE', *, *, #2207, .F. ) ;
#2233 = CARTESIAN_POINT ( 'NONE',  ( 36.35777514575907787, 25.00000000000018474, 354.7349908125917750 ) ) ;
#2234 = EDGE_CURVE ( 'NONE', #4543, #2151, #3240, .T. ) ;
#2235 = ORIENTED_EDGE ( 'NONE', *, *, #2813, .F. ) ;
#2236 = CIRCLE ( 'NONE', #3557, 40.00000000000000000 ) ;
#2237 = DIRECTION ( 'NONE',  ( -4.476705744456277327E-17, 0.000000000000000000, -1.000000000000000000 ) ) ;
#2238 = VECTOR ( 'NONE', #2468, 1000.000000000000000 ) ;
#2239 = CARTESIAN_POINT ( 'NONE',  ( -174.3534642324304116, 5.421010862427522170E-17, 552.7876087698471110 ) ) ;
#2240 = FACE_OUTER_BOUND ( 'NONE', #4377, .T. ) ;
#2241 = AXIS2_PLACEMENT_3D ( 'NONE', #956, #1476, #4822 ) ;
#2242 = ORIENTED_EDGE ( 'NONE', *, *, #1336, .T. ) ;
#2243 = ORIENTED_EDGE ( 'NONE', *, *, #4924, .T. ) ;
#2244 = VERTEX_POINT ( 'NONE', #2022 ) ;
#2245 = DIRECTION ( 'NONE',  ( -0.9955873536034882676, 5.456801509096968857E-31, -0.09383933793885568253 ) ) ;
#2246 = DIRECTION ( 'NONE',  ( -0.9998833722232040033, 6.797399803719615819E-31, 0.01527226085271964420 ) ) ;
#2247 = CARTESIAN_POINT ( 'NONE',  ( -84.02857808274407603, 84.45434506795682239, -11.99999999999995559 ) ) ;
#2248 = ORIENTED_EDGE ( 'NONE', *, *, #3821, .T. ) ;
#2249 = ORIENTED_EDGE ( 'NONE', *, *, #1211, .F. ) ;
#2250 = EDGE_CURVE ( 'NONE', #3339, #2477, #631, .T. ) ;
#2251 = EDGE_CURVE ( 'NONE', #1066, #3281, #5365, .T. ) ;
#2252 = CARTESIAN_POINT ( 'NONE',  ( -49.96441683051505578, 2.222614453595284090E-15, 542.4422122871075089 ) ) ;
#2253 = CARTESIAN_POINT ( 'NONE',  ( -315.5527284303366855, 5.957787190994857570E-15, 120.3224137463851520 ) ) ;
#2254 = EDGE_LOOP ( 'NONE', ( #4278, #3061, #448, #1632 ) ) ;
#2255 = ORIENTED_EDGE ( 'NONE', *, *, #792, .T. ) ;
#2256 = CARTESIAN_POINT ( 'NONE',  ( -360.7307227603793649, 2.222614453595284090E-15, 354.4373729494858480 ) ) ;
#2257 = EDGE_LOOP ( 'NONE', ( #3465, #808, #1925, #2697 ) ) ;
#2258 = DIRECTION ( 'NONE',  ( 5.551115123125772841E-17, -1.848892746611743135E-31, -1.000000000000000000 ) ) ;
#2259 = DIRECTION ( 'NONE',  ( 0.4205749795070160557, -0.9072577839912276954, -5.551115123125780853E-17 ) ) ;
#2260 = DIRECTION ( 'NONE',  ( -0.01527226085271972227, -2.080004339938201584E-31, -0.9998833722232041143 ) ) ;
#2261 = CLOSED_SHELL ( 'NONE', ( #2421, #4698, #4942, #90, #2946, #935, #2985, #3580, #2620, #2704, #1250 ) ) ;
#2262 = ORIENTED_EDGE ( 'NONE', *, *, #4226, .F. ) ;
#2263 = ORIENTED_EDGE ( 'NONE', *, *, #530, .F. ) ;
#2264 = CARTESIAN_POINT ( 'NONE',  ( -84.02857808274407603, 84.45434506795682239, -11.99999999999995559 ) ) ;
#2265 = DIRECTION ( 'NONE',  ( 0.09383933793885568253, -2.673190762809473730E-31, -0.9955873536034882676 ) ) ;
#2266 = DIRECTION ( 'NONE',  ( 5.551115123125772841E-17, -1.848892746611743135E-31, -1.000000000000000000 ) ) ;
#2267 = FACE_OUTER_BOUND ( 'NONE', #4746, .T. ) ;
#2268 = ORIENTED_EDGE ( 'NONE', *, *, #2524, .F. ) ;
#2269 = CIRCLE ( 'NONE', #2970, 27.43532828739476415 ) ;
#2270 = CARTESIAN_POINT ( 'NONE',  ( -84.02857808274397655, -39.54565493204319893, 152.0000000000000853 ) ) ;
#2271 = EDGE_CURVE ( 'NONE', #1449, #4228, #3267, .T. ) ;
#2272 = CARTESIAN_POINT ( 'NONE',  ( 29.77542608467487995, -25.00000000000000355, 249.2409987768023711 ) ) ;
#2273 = DIRECTION ( 'NONE',  ( 0.000000000000000000, 1.000000000000000000, 0.000000000000000000 ) ) ;
#2274 = EDGE_CURVE ( 'NONE', #1814, #1596, #3973, .T. ) ;
#2275 = DIRECTION ( 'NONE',  ( 3.204747427460360459E-31, -1.000000000000000000, 1.848892746611743354E-31 ) ) ;
#2276 = ADVANCED_FACE ( 'NONE', ( #1165 ), #2563, .T. ) ;
#2277 = FACE_BOUND ( 'NONE', #1876, .T. ) ;
#2278 = CARTESIAN_POINT ( 'NONE',  ( -1.533280346156948193, 25.00000000000018474, 488.4857301958397784 ) ) ;
#2279 = DIRECTION ( 'NONE',  ( 0.000000000000000000, 0.000000000000000000, 1.000000000000000000 ) ) ;
#2280 = ORIENTED_EDGE ( 'NONE', *, *, #4059, .F. ) ;
#2281 = ORIENTED_EDGE ( 'NONE', *, *, #1674, .F. ) ;
#2282 = FACE_OUTER_BOUND ( 'NONE', #793, .T. ) ;
#2283 = DIRECTION ( 'NONE',  ( -5.551115123125772841E-17, 1.848892746611743135E-31, 1.000000000000000000 ) ) ;
#2284 = ORIENTED_EDGE ( 'NONE', *, *, #5398, .T. ) ;
#2285 = VERTEX_POINT ( 'NONE', #2158 ) ;
#2286 = DIRECTION ( 'NONE',  ( -0.9955873536034882676, 0.000000000000000000, -0.09383933793885600172 ) ) ;
#2287 = CARTESIAN_POINT ( 'NONE',  ( -80.02857808274404761, 80.45434506795689344, -9.999999999999841904 ) ) ;
#2288 = DIRECTION ( 'NONE',  ( 5.551115123125772841E-17, -1.848892746611743135E-31, -1.000000000000000000 ) ) ;
#2289 = FACE_OUTER_BOUND ( 'NONE', #1287, .T. ) ;
#2290 = VERTEX_POINT ( 'NONE', #2095 ) ;
#2291 = SURFACE_STYLE_FILL_AREA ( #3600 ) ;
#2292 = CARTESIAN_POINT ( 'NONE',  ( -379.9227425692766360, 2.222614453595299867E-15, 174.5211340242017855 ) ) ;
#2293 = CARTESIAN_POINT ( 'NONE',  ( -156.9923520473274721, -24.99999999999981881, 556.8176423728723421 ) ) ;
#2294 = PLANE ( 'NONE',  #36 ) ;
#2295 = ADVANCED_FACE ( 'NONE', ( #2539 ), #3833, .T. ) ;
#2296 = AXIS2_PLACEMENT_3D ( 'NONE', #1306, #2986, #4660 ) ;
#2297 = CARTESIAN_POINT ( 'NONE',  ( -51.80562710762752232, 15.00000000000001421, 127.0899108387844336 ) ) ;
#2298 = AXIS2_PLACEMENT_3D ( 'NONE', #3215, #262, #3620 ) ;
#2299 = DIRECTION ( 'NONE',  ( 0.09383933793885568253, -2.673190762809473730E-31, -0.9955873536034882676 ) ) ;
#2300 = CARTESIAN_POINT ( 'NONE',  ( -72.60637664584184847, 3.252606517456513302E-16, 552.9197695054128872 ) ) ;
#2301 = PRODUCT_CONTEXT ( 'NONE', #632, 'mechanical' ) ;
#2302 = CARTESIAN_POINT ( 'NONE',  ( -342.0244061588616091, 3.740497495074990297E-15, 297.0039604601894894 ) ) ;
#2303 = CIRCLE ( 'NONE', #634, 31.50000000000114397 ) ;
#2304 = VECTOR ( 'NONE', #2787, 1000.000000000000000 ) ;
#2305 = ORIENTED_EDGE ( 'NONE', *, *, #898, .T. ) ;
#2306 = CARTESIAN_POINT ( 'NONE',  ( -339.2542556961734590, 25.00000000000018474, 239.6247169981589309 ) ) ;
#2307 = ORIENTED_EDGE ( 'NONE', *, *, #4298, .T. ) ;
#2308 = ADVANCED_FACE ( 'NONE', ( #1241 ), #2121, .T. ) ;
#2309 = DIRECTION ( 'NONE',  ( -1.219242865862094703E-16, 1.000000000000000000, -1.149200448409289593E-17 ) ) ;
#2310 = AXIS2_PLACEMENT_3D ( 'NONE', #1079, #2436, #2023 ) ;
#2311 =( NAMED_UNIT ( * ) PLANE_ANGLE_UNIT ( ) SI_UNIT ( $, .RADIAN. ) );
#2312 = VECTOR ( 'NONE', #3965, 1000.000000000000000 ) ;
#2313 = ORIENTED_EDGE ( 'NONE', *, *, #1266, .F. ) ;
#2314 = PRODUCT_DEFINITION_CONTEXT ( 'detailed design', #4845, 'design' ) ;
#2315 = TOROIDAL_SURFACE ( 'NONE', #1974, 30.50000000000110845, 1.000000000000000000 ) ;
#2316 = ORIENTED_EDGE ( 'NONE', *, *, #5428, .T. ) ;
#2317 = DIRECTION ( 'NONE',  ( -0.09383933793885568253, 2.673190762809473730E-31, 0.9955873536034882676 ) ) ;
#2318 = FACE_BOUND ( 'NONE', #4947, .T. ) ;
#2319 = CARTESIAN_POINT ( 'NONE',  ( -338.5986743560152377, 2.276824562219559311E-15, 39.80450035817695209 ) ) ;
#2320 = CARTESIAN_POINT ( 'NONE',  ( -82.68018911681723182, -17.01448963777485446, -12.00000000000006573 ) ) ;
#2321 = AXIS2_PLACEMENT_3D ( 'NONE', #2609, #491, #2167 ) ;
#2322 = PRODUCT_DEFINITION ( 'UNKNOWN', '', #928, #4515 ) ;
#2323 = AXIS2_PLACEMENT_3D ( 'NONE', #5148, #1848, #121 ) ;
#2324 = ORIENTED_EDGE ( 'NONE', *, *, #335, .T. ) ;
#2325 =( REPRESENTATION_RELATIONSHIP ('NONE','NONE', #2124, #3052 ) REPRESENTATION_RELATIONSHIP_WITH_TRANSFORMATION ( #3635 )SHAPE_REPRESENTATION_RELATIONSHIP( ) );
#2326 = FACE_OUTER_BOUND ( 'NONE', #1899, .T. ) ;
#2327 = CARTESIAN_POINT ( 'NONE',  ( 36.35777514575885760, 2.222614453595284090E-15, 354.7349908125909792 ) ) ;
#2328 = DIRECTION ( 'NONE',  ( 0.000000000000000000, 0.000000000000000000, 1.000000000000000000 ) ) ;
#2329 = DIRECTION ( 'NONE',  ( -1.000000000000000000, 0.000000000000000000, 0.000000000000000000 ) ) ;
#2330 = DIRECTION ( 'NONE',  ( -1.000000000000000000, -1.219242865862094703E-16, 0.000000000000000000 ) ) ;
#2331 = CARTESIAN_POINT ( 'NONE',  ( 36.35777514575907787, 25.00000000000018474, 354.7349908125917750 ) ) ;
#2332 = SHAPE_DEFINITION_REPRESENTATION ( #2019, #825 ) ;
#2333 = CARTESIAN_POINT ( 'NONE',  ( -12.39202333278750601, -25.00000000000000355, 98.84296066633362443 ) ) ;
#2334 = SHAPE_REPRESENTATION ( 'Induction Power Cable Socket', ( #2926 ), #5309 ) ;
#2335 = ORIENTED_EDGE ( 'NONE', *, *, #2518, .F. ) ;
#2336 = CARTESIAN_POINT ( 'NONE',  ( 4.992201166475765284, 25.00000000000018474, 252.6216919286950429 ) ) ;
#2337 = VERTEX_POINT ( 'NONE', #6 ) ;
#2338 = CARTESIAN_POINT ( 'NONE',  ( -328.0684036055322963, 2.759321206427281912E-15, 40.79703369235946298 ) ) ;
#2339 = EDGE_CURVE ( 'NONE', #1622, #1654, #4239, .T. ) ;
#2340 = CARTESIAN_POINT ( 'NONE',  ( -48.13570084519476211, 15.00000000000001421, 62.68703548022115513 ) ) ;
#2341 = EDGE_CURVE ( 'NONE', #2087, #1199, #4934, .T. ) ;
#2342 = EDGE_CURVE ( 'NONE', #3680, #3541, #4673, .T. ) ;
#2343 = ORIENTED_EDGE ( 'NONE', *, *, #961, .F. ) ;
#2344 = EDGE_CURVE ( 'NONE', #964, #577, #4843, .T. ) ;
#2345 = ORIENTED_EDGE ( 'NONE', *, *, #3804, .F. ) ;
#2346 = DIRECTION ( 'NONE',  ( -0.09383933793885537722, 2.611561004589082621E-31, 0.9955873536034883786 ) ) ;
#2347 = DIRECTION ( 'NONE',  ( 5.551115123125772841E-17, -1.848892746611743135E-31, -1.000000000000000000 ) ) ;
#2348 = FACE_OUTER_BOUND ( 'NONE', #605, .T. ) ;
#2349 = DIRECTION ( 'NONE',  ( -1.261617073437686134E-16, 1.000000000000000000, 1.232595164407830946E-31 ) ) ;
#2350 = DIRECTION ( 'NONE',  ( 5.551115123125772841E-17, -1.848892746611743135E-31, -1.000000000000000000 ) ) ;
#2351 = ORIENTED_EDGE ( 'NONE', *, *, #3893, .T. ) ;
#2352 = AXIS2_PLACEMENT_3D ( 'NONE', #2968, #1346, #468 ) ;
#2353 =( NAMED_UNIT ( * ) PLANE_ANGLE_UNIT ( ) SI_UNIT ( $, .RADIAN. ) );
#2354 = CYLINDRICAL_SURFACE ( 'NONE', #4517, 14.00000000000002665 ) ;
#2355 = CARTESIAN_POINT ( 'NONE',  ( -72.60637664584184847, 3.252606517456513302E-16, 552.9197695054128872 ) ) ;
#2356 = DIRECTION ( 'NONE',  ( 5.551115123125772841E-17, -1.848892746611743135E-31, -1.000000000000000000 ) ) ;
#2357 = AXIS2_PLACEMENT_3D ( 'NONE', #4937, #1178, #4538 ) ;
#2358 = FACE_OUTER_BOUND ( 'NONE', #1774, .T. ) ;
#2359 = DIRECTION ( 'NONE',  ( 0.000000000000000000, 0.000000000000000000, 1.000000000000000000 ) ) ;
#2360 = ADVANCED_FACE ( 'NONE', ( #4192, #858 ), #445, .T. ) ;
#2361 = CARTESIAN_POINT ( 'NONE',  ( 10.82492224058160879, 25.00000000000018474, 312.2165827548579387 ) ) ;
#2362 = CARTESIAN_POINT ( 'NONE',  ( -285.5643670724624599, -25.00000000000003197, 494.2304181244473966 ) ) ;
#2363 = CARTESIAN_POINT ( 'NONE',  ( 33.59898979596731294, 5.421010862427522170E-17, 384.0431050523496310 ) ) ;
#2364 = TOROIDAL_SURFACE ( 'NONE', #5429, 28.50000000000115463, 1.000000000000000000 ) ;
#2365 = ORIENTED_EDGE ( 'NONE', *, *, #1753, .T. ) ;
#2366 = CARTESIAN_POINT ( 'NONE',  ( -367.0460729392618191, 25.00000000000018474, 268.0688838304706678 ) ) ;
#2367 = ORIENTED_EDGE ( 'NONE', *, *, #1736, .T. ) ;
#2368 = CARTESIAN_POINT ( 'NONE',  ( 137.9714219172562366, -25.54565493204319182, -5.551115123125782702E-14 ) ) ;
#2369 = LINE ( 'NONE', #4458, #2407 ) ;
#2370 = ADVANCED_FACE ( 'NONE', ( #5055 ), #3320, .F. ) ;
#2371 = ORIENTED_EDGE ( 'NONE', *, *, #5089, .T. ) ;
#2372 = UNCERTAINTY_MEASURE_WITH_UNIT (LENGTH_MEASURE( 1.000000000000000082E-05 ), #4402, 'distance_accuracy_value', 'NONE');
#2373 = ADVANCED_FACE ( 'NONE', ( #3402, #1298 ), #4141, .F. ) ;
#2374 = ORIENTED_EDGE ( 'NONE', *, *, #971, .F. ) ;
#2375 = LINE ( 'NONE', #1879, #566 ) ;
#2376 = CARTESIAN_POINT ( 'NONE',  ( -85.27857808274418971, -21.54565493204320248, -2.000000000000002220 ) ) ;
#2377 = CARTESIAN_POINT ( 'NONE',  ( -361.0769802293077646, 2.222614453595279751E-15, 36.68136974599871536 ) ) ;
#2378 = DIRECTION ( 'NONE',  ( 0.09383933793885537722, -2.626968444144180508E-31, -0.9955873536034883786 ) ) ;
#2379 = DIRECTION ( 'NONE',  ( 0.9955873536034882676, -5.498835694391114214E-31, 0.09383933793885514130 ) ) ;
#2380 = ORIENTED_EDGE ( 'NONE', *, *, #298, .F. ) ;
#2381 = DIRECTION ( 'NONE',  ( -0.01527226085271972227, -2.080004339938201146E-31, -0.9998833722232041143 ) ) ;
#2382 = CARTESIAN_POINT ( 'NONE',  ( 132.2270686671743647, -26.49739520581860219, -9.999999999999953815 ) ) ;
#2383 = CARTESIAN_POINT ( 'NONE',  ( -57.28677601057280100, 3.252606517456513302E-16, 546.4981013186296650 ) ) ;
#2384 = LINE ( 'NONE', #1248, #1620 ) ;
#2385 = PLANE ( 'NONE',  #3638 ) ;
#2386 = EDGE_CURVE ( 'NONE', #2244, #3719, #1340, .T. ) ;
#2387 = FACE_OUTER_BOUND ( 'NONE', #4633, .T. ) ;
#2388 = CARTESIAN_POINT ( 'NONE',  ( -223.9642223310802649, 24.99999999999997158, 534.3227077390027944 ) ) ;
#2389 = CARTESIAN_POINT ( 'NONE',  ( -72.60637664584220374, -24.99999999999981881, 552.9197695054134556 ) ) ;
#2390 = CARTESIAN_POINT ( 'NONE',  ( -74.02857808274409024, -21.54565493204321669, -12.00000000000001066 ) ) ;
#2391 = AXIS2_PLACEMENT_3D ( 'NONE', #2929, #1657, #2166 ) ;
#2392 = ORIENTED_EDGE ( 'NONE', *, *, #1203, .F. ) ;
#2393 = CARTESIAN_POINT ( 'NONE',  ( 0.07030049710132768581, 1.843143693225357538E-15, 219.5055207296747710 ) ) ;
#2394 = ORIENTED_EDGE ( 'NONE', *, *, #159, .T. ) ;
#2395 = CIRCLE ( 'NONE', #19, 27.50000000000126832 ) ;
#2396 = DIRECTION ( 'NONE',  ( -0.9955873536034882676, 5.502656983963203831E-31, -0.09383933793885550212 ) ) ;
#2397 = CARTESIAN_POINT ( 'NONE',  ( 119.2387771779189478, -14.99999999999998579, 167.0961341013325523 ) ) ;
#2398 = AXIS2_PLACEMENT_3D ( 'NONE', #2368, #5245, #1485 ) ;
#2399 = EDGE_LOOP ( 'NONE', ( #1991, #3888 ) ) ;
#2400 = AXIS2_PLACEMENT_3D ( 'NONE', #3892, #4310, #202 ) ;
#2401 = AXIS2_PLACEMENT_3D ( 'NONE', #5066, #4282, #2549 ) ;
#2402 = ORIENTED_EDGE ( 'NONE', *, *, #2075, .T. ) ;
#2403 = LINE ( 'NONE', #232, #2304 ) ;
#2404 = DIRECTION ( 'NONE',  ( 0.09383933793885568253, -2.673190762809473730E-31, -0.9955873536034882676 ) ) ;
#2405 = DIRECTION ( 'NONE',  ( 0.09383933793885537722, -2.626968444144180508E-31, -0.9955873536034883786 ) ) ;
#2406 = CARTESIAN_POINT ( 'NONE',  ( 0.000000000000000000, 0.000000000000000000, 0.000000000000000000 ) ) ;
#2407 = VECTOR ( 'NONE', #4049, 1000.000000000000114 ) ;
#2408 = AXIS2_PLACEMENT_3D ( 'NONE', #1885, #4841, #5231 ) ;
#2409 = FACE_OUTER_BOUND ( 'NONE', #2805, .T. ) ;
#2410 = ORIENTED_EDGE ( 'NONE', *, *, #5046, .F. ) ;
#2411 = AXIS2_PLACEMENT_3D ( 'NONE', #2869, #772, #2969 ) ;
#2412 = DIRECTION ( 'NONE',  ( -1.000000000000000000, 0.000000000000000000, 0.000000000000000000 ) ) ;
#2413 = VECTOR ( 'NONE', #3248, 1000.000000000000114 ) ;
#2414 = DIRECTION ( 'NONE',  ( 0.9955873536034882676, -5.475514420260265162E-31, 0.09383933793885552987 ) ) ;
#2415 = LINE ( 'NONE', #2029, #5211 ) ;
#2416 = VECTOR ( 'NONE', #4308, 1000.000000000000000 ) ;
#2417 = EDGE_CURVE ( 'NONE', #577, #4350, #2736, .T. ) ;
#2418 = SURFACE_STYLE_FILL_AREA ( #733 ) ;
#2419 = EDGE_CURVE ( 'NONE', #1042, #5024, #3628, .T. ) ;
#2420 = AXIS2_PLACEMENT_3D ( 'NONE', #5320, #4498, #1583 ) ;
#2421 = ADVANCED_FACE ( 'NONE', ( #4169 ), #4551, .F. ) ;
#2422 = DIRECTION ( 'NONE',  ( 1.000000000000000000, -3.759415251443877379E-31, 5.551115123125772841E-17 ) ) ;
#2423 = CARTESIAN_POINT ( 'NONE',  ( -342.0170653153610374, 25.00000000000018474, 268.9367132353194734 ) ) ;
#2424 = CARTESIAN_POINT ( 'NONE',  ( -320.6447527397745034, -25.00000000000003197, 453.8399743637903612 ) ) ;
#2425 = VERTEX_POINT ( 'NONE', #2874 ) ;
#2426 = CARTESIAN_POINT ( 'NONE',  ( 9.699276322990584731, 1.572093150103981429E-15, 297.8714164406039799 ) ) ;
#2427 = VERTEX_POINT ( 'NONE', #3753 ) ;
#2428 = PLANE ( 'NONE',  #2136 ) ;
#2429 = CARTESIAN_POINT ( 'NONE',  ( 96.73877717791896202, -14.99999999999998579, 131.6034880481681171 ) ) ;
#2430 = ORIENTED_EDGE ( 'NONE', *, *, #3925, .F. ) ;
#2431 = ORIENTED_EDGE ( 'NONE', *, *, #78, .F. ) ;
#2432 = DIRECTION ( 'NONE',  ( 0.9955873536034882676, -5.498529991225536465E-31, 0.09383933793885551600 ) ) ;
#2433 = CARTESIAN_POINT ( 'NONE',  ( -345.9181427152443007, 2.222614453595284090E-15, 117.4603139392499429 ) ) ;
#2434 = CARTESIAN_POINT ( 'NONE',  ( -330.4329412795323719, 2.816687638039060658E-15, 198.2700196465188753 ) ) ;
#2435 = EDGE_CURVE ( 'NONE', #4710, #774, #2486, .T. ) ;
#2436 = DIRECTION ( 'NONE',  ( 0.09383933793885568253, -2.673190762809473730E-31, -0.9955873536034882676 ) ) ;
#2437 =( BOUNDED_SURFACE ( )  B_SPLINE_SURFACE ( 3, 3, ( 
 ( #2229, #1919, #4015, #3110, #576, #1457, #4781, #3935, #3606, #4395, #1041, #1479, #3958, #1017, #2716, #2664, #987, #3906, #216, #137, #3140, #2300, #4857, #5214, #5160, #2694, #598, #4422, #5264, #3985, #547, #1500, #3081, #4751, #5182, #1063, #4347, #164 ),
 ( #3167, #1094, #2739, #655, #186, #3581, #4371, #1836, #2331, #245, #3551, #3526, #5238, #1424, #2278, #3197, #4826, #1863, #2005, #790, #4126, #2826, #383, #763, #271, #5352, #2450, #3664, #2388, #2886, #4040, #5294, #3686, #4539, #703, #5406, #4939, #356 ),
 ( #1640, #4154, #4071, #3252, #4565, #2773, #2361, #1981, #2034, #4971, #3311, #4449, #4104, #304, #4502, #3225, #1149, #4478, #1618, #2060, #1179, #1948, #2799, #1537, #3634, #2863, #5323, #1587, #1564, #4884, #1122, #3335, #4909, #737, #3709, #1209, #2423, #332 ),
 ( #2474, #3278, #4991, #5379, #3743, #678, #3818, #5012, #1312, #2613, #49, #3357, #1255, #2170, #2108, #3781, #2197, #819, #411, #5070, #2939, #517, #17, #2141, #3764, #4640, #1719, #5096, #2992, #1338, #3870, #932, #4614, #2503, #5043, #1661, #4665, #2084 ),
 ( #848, #3414, #900, #2580, #3025, #4232, #2906, #4587, #2527, #4263, #3440, #4183, #4286, #100, #1686, #4206, #494, #3386, #433, #1778, #3844, #76, #1748, #871, #1282, #4699, #2963, #2551, #4612, #3470, #457, #1232, #1452, #240, #594, #1809, #4726, #3522 ),
 ( #3103, #210, #1831, #5155, #2272, #3952, #3134, #1475, #2689, #1373, #3054, #134, #181, #1890, #955, #2731, #4821, #3932, #1399, #1856, #157, #4748, #4414, #5208, #3543, #2293, #4774, #5179, #4800, #3497, #3077, #2636, #1037, #4314, #2712, #4390, #1914, #614 ),
 ( #572, #981, #5234, #542, #2224, #4367, #3977, #2659, #2327, #3576, #3163, #1419, #1057, #3901, #649, #5130, #4011, #4339, #1014, #2252, #2383, #2355, #2028, #3705, #2823, #673, #2856, #3626, #4880, #1201, #326, #4065, #4497, #1610, #4932, #3659, #2882, #1582 ) ),
 .UNSPECIFIED., .T., .F., .T. ) 
 B_SPLINE_SURFACE_WITH_KNOTS ( ( 4, 3, 4 ),
 ( 4, 2, 2, 2, 2, 2, 2, 2, 2, 2, 2, 2, 2, 2, 2, 2, 2, 2, 4 ),
 ( 0.000000000000000000, 0.5000000000000000000, 1.000000000000000000 ),
 ( 0.000000000000000000, 0.1028767157186024211, 0.2057534314372048423, 0.2571917892965060459, 0.3086301471558072773, 0.3600685050151084532, 0.4115068628744096846, 0.4558387458985032614, 0.4780046874105500776, 0.5001706289225968938, 0.5231687412733679876, 0.5461668536241390814, 0.5921630783256812691, 0.6381593030272234568, 0.6841555277287657555, 0.7631166457965743444, 0.8420777638643828222, 0.9210388819321914111, 1.000000000000000000 ),
 .UNSPECIFIED. ) 
 GEOMETRIC_REPRESENTATION_ITEM ( )  RATIONAL_B_SPLINE_SURFACE ( (
 ( 1.000000000000000000, 1.000000000000000000, 1.000000000000000000, 1.000000000000000000, 1.000000000000000000, 1.000000000000000000, 1.000000000000000000, 1.000000000000000000, 1.000000000000000000, 1.000000000000000000, 1.000000000000000000, 1.000000000000000000, 1.000000000000000000, 1.000000000000000000, 1.000000000000000000, 1.000000000000000000, 1.000000000000000000, 1.000000000000000000, 1.000000000000000000, 1.000000000000000000, 1.000000000000000000, 1.000000000000000000, 1.000000000000000000, 1.000000000000000000, 1.000000000000000000, 1.000000000000000000, 1.000000000000000000, 1.000000000000000000, 1.000000000000000000, 1.000000000000000000, 1.000000000000000000, 1.000000000000000000, 1.000000000000000000, 1.000000000000000000, 1.000000000000000000, 1.000000000000000000, 1.000000000000000000, 1.000000000000000000),
 ( 0.3333333333333333703, 0.3333333333333333703, 0.3333333333333333703, 0.3333333333333333703, 0.3333333333333333703, 0.3333333333333333703, 0.3333333333333333703, 0.3333333333333333703, 0.3333333333333333703, 0.3333333333333333703, 0.3333333333333333703, 0.3333333333333333703, 0.3333333333333333703, 0.3333333333333333703, 0.3333333333333333703, 0.3333333333333333703, 0.3333333333333333703, 0.3333333333333333703, 0.3333333333333333703, 0.3333333333333333703, 0.3333333333333333703, 0.3333333333333333703, 0.3333333333333333703, 0.3333333333333333703, 0.3333333333333333703, 0.3333333333333333703, 0.3333333333333333703, 0.3333333333333333703, 0.3333333333333333703, 0.3333333333333333703, 0.3333333333333333703, 0.3333333333333333703, 0.3333333333333333703, 0.3333333333333333703, 0.3333333333333333703, 0.3333333333333333703, 0.3333333333333333703, 0.3333333333333333703),
 ( 0.3333333333333333703, 0.3333333333333333703, 0.3333333333333333703, 0.3333333333333333703, 0.3333333333333333703, 0.3333333333333333703, 0.3333333333333333703, 0.3333333333333333703, 0.3333333333333333703, 0.3333333333333333703, 0.3333333333333333703, 0.3333333333333333703, 0.3333333333333333703, 0.3333333333333333703, 0.3333333333333333703, 0.3333333333333333703, 0.3333333333333333703, 0.3333333333333333703, 0.3333333333333333703, 0.3333333333333333703, 0.3333333333333333703, 0.3333333333333333703, 0.3333333333333333703, 0.3333333333333333703, 0.3333333333333333703, 0.3333333333333333703, 0.3333333333333333703, 0.3333333333333333703, 0.3333333333333333703, 0.3333333333333333703, 0.3333333333333333703, 0.3333333333333333703, 0.3333333333333333703, 0.3333333333333333703, 0.3333333333333333703, 0.3333333333333333703, 0.3333333333333333703, 0.3333333333333333703),
 ( 1.000000000000000000, 1.000000000000000000, 1.000000000000000000, 1.000000000000000000, 1.000000000000000000, 1.000000000000000000, 1.000000000000000000, 1.000000000000000000, 1.000000000000000000, 1.000000000000000000, 1.000000000000000000, 1.000000000000000000, 1.000000000000000000, 1.000000000000000000, 1.000000000000000000, 1.000000000000000000, 1.000000000000000000, 1.000000000000000000, 1.000000000000000000, 1.000000000000000000, 1.000000000000000000, 1.000000000000000000, 1.000000000000000000, 1.000000000000000000, 1.000000000000000000, 1.000000000000000000, 1.000000000000000000, 1.000000000000000000, 1.000000000000000000, 1.000000000000000000, 1.000000000000000000, 1.000000000000000000, 1.000000000000000000, 1.000000000000000000, 1.000000000000000000, 1.000000000000000000, 1.000000000000000000, 1.000000000000000000),
 ( 0.3333333333333333703, 0.3333333333333333703, 0.3333333333333333703, 0.3333333333333333703, 0.3333333333333333703, 0.3333333333333333703, 0.3333333333333333703, 0.3333333333333333703, 0.3333333333333333703, 0.3333333333333333703, 0.3333333333333333703, 0.3333333333333333703, 0.3333333333333333703, 0.3333333333333333703, 0.3333333333333333703, 0.3333333333333333703, 0.3333333333333333703, 0.3333333333333333703, 0.3333333333333333703, 0.3333333333333333703, 0.3333333333333333703, 0.3333333333333333703, 0.3333333333333333703, 0.3333333333333333703, 0.3333333333333333703, 0.3333333333333333703, 0.3333333333333333703, 0.3333333333333333703, 0.3333333333333333703, 0.3333333333333333703, 0.3333333333333333703, 0.3333333333333333703, 0.3333333333333333703, 0.3333333333333333703, 0.3333333333333333703, 0.3333333333333333703, 0.3333333333333333703, 0.3333333333333333703),
 ( 0.3333333333333333703, 0.3333333333333333703, 0.3333333333333333703, 0.3333333333333333703, 0.3333333333333333703, 0.3333333333333333703, 0.3333333333333333703, 0.3333333333333333703, 0.3333333333333333703, 0.3333333333333333703, 0.3333333333333333703, 0.3333333333333333703, 0.3333333333333333703, 0.3333333333333333703, 0.3333333333333333703, 0.3333333333333333703, 0.3333333333333333703, 0.3333333333333333703, 0.3333333333333333703, 0.3333333333333333703, 0.3333333333333333703, 0.3333333333333333703, 0.3333333333333333703, 0.3333333333333333703, 0.3333333333333333703, 0.3333333333333333703, 0.3333333333333333703, 0.3333333333333333703, 0.3333333333333333703, 0.3333333333333333703, 0.3333333333333333703, 0.3333333333333333703, 0.3333333333333333703, 0.3333333333333333703, 0.3333333333333333703, 0.3333333333333333703, 0.3333333333333333703, 0.3333333333333333703),
 ( 1.000000000000000000, 1.000000000000000000, 1.000000000000000000, 1.000000000000000000, 1.000000000000000000, 1.000000000000000000, 1.000000000000000000, 1.000000000000000000, 1.000000000000000000, 1.000000000000000000, 1.000000000000000000, 1.000000000000000000, 1.000000000000000000, 1.000000000000000000, 1.000000000000000000, 1.000000000000000000, 1.000000000000000000, 1.000000000000000000, 1.000000000000000000, 1.000000000000000000, 1.000000000000000000, 1.000000000000000000, 1.000000000000000000, 1.000000000000000000, 1.000000000000000000, 1.000000000000000000, 1.000000000000000000, 1.000000000000000000, 1.000000000000000000, 1.000000000000000000, 1.000000000000000000, 1.000000000000000000, 1.000000000000000000, 1.000000000000000000, 1.000000000000000000, 1.000000000000000000, 1.000000000000000000, 1.000000000000000000) ) ) 
 REPRESENTATION_ITEM ( '' )  SURFACE ( )  );
#2438 = APPLICATION_CONTEXT ( 'automotive_design' ) ;
#2439 = CARTESIAN_POINT ( 'NONE',  ( 128.7214219172562366, -21.54565493204319182, -26.84924240491753977 ) ) ;
#2440 = ORIENTED_EDGE ( 'NONE', *, *, #1746, .F. ) ;
#2441 = ORIENTED_EDGE ( 'NONE', *, *, #2578, .F. ) ;
#2442 = DIRECTION ( 'NONE',  ( 0.09383933793885568253, -2.673190762809473730E-31, -0.9955873536034882676 ) ) ;
#2443 = AXIS2_PLACEMENT_3D ( 'NONE', #5206, #3899, #613 ) ;
#2444 = CARTESIAN_POINT ( 'NONE',  ( -346.1058213911226176, 0.000000000000000000, 119.4514886464559424 ) ) ;
#2445 = CARTESIAN_POINT ( 'NONE',  ( 6.123233995736766085E-15, 80.00000000000000000, 50.00000000000000000 ) ) ;
#2446 = CARTESIAN_POINT ( 'NONE',  ( -80.02857808274418971, -21.54565493204321669, -2.000000000000001776 ) ) ;
#2447 = CIRCLE ( 'NONE', #1912, 31.50000000000114397 ) ;
#2448 = ADVANCED_FACE ( 'NONE', ( #4737 ), #4681, .F. ) ;
#2449 = DIRECTION ( 'NONE',  ( -0.4205749795070158337, -0.9072577839912276954, 0.000000000000000000 ) ) ;
#2450 = CARTESIAN_POINT ( 'NONE',  ( -174.3534642324312358, 25.00000000000018474, 552.7876087698487027 ) ) ;
#2451 = CARTESIAN_POINT ( 'NONE',  ( -207.8397519515722252, -25.00000000000003197, 541.5412455041529256 ) ) ;
#2452 = EDGE_CURVE ( 'NONE', #4297, #1438, #1794, .T. ) ;
#2453 = ORIENTED_EDGE ( 'NONE', *, *, #5046, .T. ) ;
#2454 = CARTESIAN_POINT ( 'NONE',  ( -39.32426838448843398, 3.740497495074990297E-15, 499.4571537926191240 ) ) ;
#2455 = ORIENTED_EDGE ( 'NONE', *, *, #1403, .F. ) ;
#2456 = CARTESIAN_POINT ( 'NONE',  ( -0.6802310551622114954, 2.222614453595284090E-15, 47.14310755735262859 ) ) ;
#2457 = EDGE_CURVE ( 'NONE', #281, #4617, #4328, .T. ) ;
#2458 = EDGE_LOOP ( 'NONE', ( #439, #2617, #1265 ) ) ;
#2459 = EDGE_LOOP ( 'NONE', ( #4020, #1573 ) ) ;
#2460 = PRODUCT ( 'Induction Power Cable Socket', 'Induction Power Cable Socket', '', ( #2301 ) ) ;
#2461 = FACE_OUTER_BOUND ( 'NONE', #714, .T. ) ;
#2462 = DIRECTION ( 'NONE',  ( -1.261617073437686134E-16, 1.000000000000000000, 1.232595164407830946E-31 ) ) ;
#2463 = DIRECTION ( 'NONE',  ( -1.000000000000000000, 0.000000000000000000, 0.000000000000000000 ) ) ;
#2464 = CARTESIAN_POINT ( 'NONE',  ( -60.76122282208098824, -14.99999999999998579, 167.0961341013325523 ) ) ;
#2465 = DIRECTION ( 'NONE',  ( 1.000000000000000000, -5.777789833161702304E-31, 0.000000000000000000 ) ) ;
#2466 = ORIENTED_EDGE ( 'NONE', *, *, #5358, .T. ) ;
#2467 = ORIENTED_EDGE ( 'NONE', *, *, #3329, .T. ) ;
#2468 = DIRECTION ( 'NONE',  ( -0.09383933793885568253, 2.673190762809473730E-31, 0.9955873536034882676 ) ) ;
#2469 = DIRECTION ( 'NONE',  ( 0.9955873536034882676, -5.502656983963330823E-31, 0.09383933793885547436 ) ) ;
#2470 = ADVANCED_BREP_SHAPE_REPRESENTATION ( '', ( #1308, #2926 ), #724 ) ;
#2471 = LINE ( 'NONE', #1118, #1702 ) ;
#2472 = SURFACE_SIDE_STYLE ('',( #2904 ) ) ;
#2473 = DIRECTION ( 'NONE',  ( 1.000000000000000000, 0.000000000000000000, 0.000000000000000000 ) ) ;
#2474 = CARTESIAN_POINT ( 'NONE',  ( -13.17877320795268759, 1.897353801849632760E-15, 47.33401081801291355 ) ) ;
#2475 = CARTESIAN_POINT ( 'NONE',  ( -57.28677601057306390, -24.99999999999981881, 546.4981013186294376 ) ) ;
#2476 = VERTEX_POINT ( 'NONE', #5167 ) ;
#2477 = VERTEX_POINT ( 'NONE', #1760 ) ;
#2478 = VECTOR ( 'NONE', #1770, 999.9999999999998863 ) ;
#2479 = DIRECTION ( 'NONE',  ( 0.9998833722232041143, -6.779273404243022909E-31, -0.01527226085271993737 ) ) ;
#2480 = DIRECTION ( 'NONE',  ( -5.551115123125772841E-17, 1.848892746611743135E-31, 1.000000000000000000 ) ) ;
#2481 = VECTOR ( 'NONE', #1324, 1000.000000000000114 ) ;
#2482 = EDGE_CURVE ( 'NONE', #5024, #1678, #1097, .T. ) ;
#2483 = ORIENTED_EDGE ( 'NONE', *, *, #3804, .T. ) ;
#2484 = ORIENTED_EDGE ( 'NONE', *, *, #5162, .F. ) ;
#2485 = EDGE_CURVE ( 'NONE', #4236, #3749, #5113, .T. ) ;
#2486 = CIRCLE ( 'NONE', #108, 6.000000000000032863 ) ;
#2487 = CARTESIAN_POINT ( 'NONE',  ( 106.6132552010327288, 15.00000000000001421, 71.50523272244407735 ) ) ;
#2488 = DIRECTION ( 'NONE',  ( 1.000000000000000000, -3.759415251443877379E-31, 5.551115123125772841E-17 ) ) ;
#2489 = DIRECTION ( 'NONE',  ( 0.01527226085271972227, 2.095411779493299033E-31, 0.9998833722232041143 ) ) ;
#2490 = ORIENTED_EDGE ( 'NONE', *, *, #1377, .F. ) ;
#2491 = CIRCLE ( 'NONE', #1866, 5.250000000000004441 ) ;
#2492 = EDGE_LOOP ( 'NONE', ( #853, #2440, #392, #492 ) ) ;
#2493 = CARTESIAN_POINT ( 'NONE',  ( 96.73877717791896202, 0.000000000000000000, 67.09613410133256650 ) ) ;
#2494 = CARTESIAN_POINT ( 'NONE',  ( -80.02857808274401918, 80.45434506795689344, -12.00000000000001066 ) ) ;
#2495 = CARTESIAN_POINT ( 'NONE',  ( -82.68018911681716077, -17.01448963777485446, -9.999999999999953815 ) ) ;
#2496 = EDGE_CURVE ( 'NONE', #4831, #3541, #4256, .T. ) ;
#2497 = AXIS2_PLACEMENT_3D ( 'NONE', #1110, #1140, #4056 ) ;
#2498 = DIRECTION ( 'NONE',  ( -1.000000000000000000, 0.000000000000000000, 0.000000000000000000 ) ) ;
#2499 = B_SPLINE_CURVE_WITH_KNOTS ( 'NONE', 3,
 ( #2577, #4990, #381, #1231, #4153, #817, #5431, #2502, #3385, #2059, #5042, #4182, #432, #4639, #2139, #3356, #2083, #4262, #5405, #2905, #870, #3334, #1639, #493, #2169, #5011, #2550, #3023, #3843, #3763, #2938, #75, #410, #1253, #4613, #3817, #4664, #2991 ),
 .UNSPECIFIED., .F., .F.,
 ( 4, 2, 2, 2, 2, 2, 2, 2, 2, 2, 2, 2, 2, 2, 2, 2, 2, 2, 4 ),
 ( 0.000000000000000000, 0.1028767157186024211, 0.2057534314372048423, 0.2571917892965060459, 0.3086301471558072773, 0.3600685050151084532, 0.4115068628744096846, 0.4558387458985032614, 0.4780046874105500776, 0.5001706289225968938, 0.5231687412733679876, 0.5461668536241390814, 0.5921630783256812691, 0.6381593030272234568, 0.6841555277287657555, 0.7631166457965743444, 0.8420777638643828222, 0.9210388819321914111, 1.000000000000000000 ),
 .UNSPECIFIED. ) ;
#2500 = CIRCLE ( 'NONE', #999, 4.382543221487789964 ) ;
#2501 = CIRCLE ( 'NONE', #125, 5.250000000000031974 ) ;
#2502 = CARTESIAN_POINT ( 'NONE',  ( 11.65205807320734976, 3.740497495074990297E-15, 340.0738060255405912 ) ) ;
#2503 = CARTESIAN_POINT ( 'NONE',  ( -330.1866567701584927, 3.740497495074990297E-15, 374.2973685668102917 ) ) ;
#2504 = CYLINDRICAL_SURFACE ( 'NONE', #390, 21.00000000000012790 ) ;
#2505 = CIRCLE ( 'NONE', #831, 28.50000000000127898 ) ;
#2506 = AXIS2_PLACEMENT_3D ( 'NONE', #2883, #786, #1174 ) ;
#2507 = PRODUCT_DEFINITION_SHAPE ( 'NONE', 'NONE',  #5433 ) ;
#2508 = EDGE_LOOP ( 'NONE', ( #139, #972 ) ) ;
#2509 = CARTESIAN_POINT ( 'NONE',  ( 127.9714219172562508, -21.54565493204319182, -12.00000000000006573 ) ) ;
#2510 = FACE_OUTER_BOUND ( 'NONE', #2956, .T. ) ;
#2511 = ORIENTED_EDGE ( 'NONE', *, *, #2031, .T. ) ;
#2512 = EDGE_CURVE ( 'NONE', #774, #556, #3486, .T. ) ;
#2513 = CARTESIAN_POINT ( 'NONE',  ( -78.28422483266226095, 85.40608534173227895, -10.00000000000006395 ) ) ;
#2514 = DIRECTION ( 'NONE',  ( -0.9955873536034883786, 5.496925049605202091E-31, -0.09383933793885522456 ) ) ;
#2515 = EDGE_CURVE ( 'NONE', #4297, #3915, #2395, .T. ) ;
#2516 = CARTESIAN_POINT ( 'NONE',  ( -351.6990976162155107, 2.276824562219559311E-15, 238.4517252739237847 ) ) ;
#2517 = CARTESIAN_POINT ( 'NONE',  ( -321.2769280446073026, 3.850615185981194977E-15, 181.0532423161974975 ) ) ;
#2518 = EDGE_CURVE ( 'NONE', #2126, #342, #4073, .T. ) ;
#2519 = EDGE_CURVE ( 'NONE', #3766, #4657, #4849, .T. ) ;
#2520 = ORIENTED_EDGE ( 'NONE', *, *, #2981, .F. ) ;
#2521 = VERTEX_POINT ( 'NONE', #2390 ) ;
#2522 = CARTESIAN_POINT ( 'NONE',  ( -0.6802310551622114954, 2.222614453595284090E-15, 47.14310755735262859 ) ) ;
#2523 = LINE ( 'NONE', #71, #1335 ) ;
#2524 = EDGE_CURVE ( 'NONE', #2290, #229, #4887, .T. ) ;
#2525 = CARTESIAN_POINT ( 'NONE',  ( -344.4167133082243595, 2.222614453595284090E-15, 101.5309162815936048 ) ) ;
#2526 = LINE ( 'NONE', #456, #2534 ) ;
#2527 = CARTESIAN_POINT ( 'NONE',  ( 11.35554381054933160, -24.99999999999981881, 353.5846600851155017 ) ) ;
#2528 = DIRECTION ( 'NONE',  ( 5.551115123125772841E-17, -1.848892746611743135E-31, -1.000000000000000000 ) ) ;
#2529 = AXIS2_PLACEMENT_3D ( 'NONE', #2538, #1193, #3698 ) ;
#2530 = CLOSED_SHELL ( 'NONE', ( #2276, #4948, #5328, #2848, #2912, #3353, #658, #1134, #235, #3956 ) ) ;
#2531 = ORIENTED_EDGE ( 'NONE', *, *, #1439, .T. ) ;
#2532 = DIRECTION ( 'NONE',  ( 0.09383933793885568253, -2.673190762809473730E-31, -0.9955873536034882676 ) ) ;
#2533 = FILL_AREA_STYLE ('',( #438 ) ) ;
#2534 = VECTOR ( 'NONE', #4205, 1000.000000000000000 ) ;
#2535 = ORIENTED_EDGE ( 'NONE', *, *, #5158, .T. ) ;
#2536 = LINE ( 'NONE', #1731, #1073 ) ;
#2537 = LINE ( 'NONE', #4651, #990 ) ;
#2538 = CARTESIAN_POINT ( 'NONE',  ( -346.0119820531830328, 0.000000000000000000, 118.4559012928528858 ) ) ;
#2539 = FACE_OUTER_BOUND ( 'NONE', #1691, .T. ) ;
#2540 = EDGE_CURVE ( 'NONE', #4195, #3075, #1983, .T. ) ;
#2541 = PLANE ( 'NONE',  #1437 ) ;
#2542 = ORIENTED_EDGE ( 'NONE', *, *, #2274, .F. ) ;
#2543 = EDGE_LOOP ( 'NONE', ( #946, #4998 ) ) ;
#2544 = ORIENTED_EDGE ( 'NONE', *, *, #1787, .T. ) ;
#2545 = PLANE ( 'NONE',  #308 ) ;
#2546 = CARTESIAN_POINT ( 'NONE',  ( 113.4038502097781276, 15.00000000000001421, 172.0544138201894668 ) ) ;
#2547 = DIRECTION ( 'NONE',  ( 5.551115123125772841E-17, -1.848892746611743135E-31, -1.000000000000000000 ) ) ;
#2548 = PRODUCT_DEFINITION_SHAPE ( 'NONE', 'NONE',  #2160 ) ;
#2549 = DIRECTION ( 'NONE',  ( -1.000000000000000000, 0.000000000000000000, -7.228014483236656373E-17 ) ) ;
#2550 = CARTESIAN_POINT ( 'NONE',  ( -167.9289969670494997, 3.740497495074990297E-15, 528.5729890193238134 ) ) ;
#2551 = CARTESIAN_POINT ( 'NONE',  ( -198.3455225866221667, -25.00000000000003197, 518.3576047634796851 ) ) ;
#2552 = CARTESIAN_POINT ( 'NONE',  ( -364.1439395362591540, 2.222614453595284090E-15, 237.2787335496894343 ) ) ;
#2553 = VECTOR ( 'NONE', #2462, 1000.000000000000000 ) ;
#2554 = VERTEX_POINT ( 'NONE', #5109 ) ;
#2555 = ORIENTED_EDGE ( 'NONE', *, *, #5219, .F. ) ;
#2556 = DIRECTION ( 'NONE',  ( -0.9955873536034882676, 5.452307672560245432E-31, -0.09383933793885568253 ) ) ;
#2557 = CARTESIAN_POINT ( 'NONE',  ( -80.02857808274413287, 80.45434506795689344, -26.84924240491753977 ) ) ;
#2558 = EDGE_LOOP ( 'NONE', ( #5193, #5045, #2249, #1329 ) ) ;
#2559 = CARTESIAN_POINT ( 'NONE',  ( -323.7051989975983588, 2.222614453595284090E-15, 41.20828864675230108 ) ) ;
#2560 = PLANE ( 'NONE',  #5376 ) ;
#2561 = CARTESIAN_POINT ( 'NONE',  ( -86.97194166595193110, -24.99999999999981881, 531.0655262460722952 ) ) ;
#2562 = SURFACE_STYLE_FILL_AREA ( #4679 ) ;
#2563 = CYLINDRICAL_SURFACE ( 'NONE', #3457, 14.00000000000002665 ) ;
#2564 = CARTESIAN_POINT ( 'NONE',  ( -353.5191290882918338, 0.000000000000000000, 198.1028895811327573 ) ) ;
#2565 = AXIS2_PLACEMENT_3D ( 'NONE', #2000, #4474, #2414 ) ;
#2566 = ORIENTED_EDGE ( 'NONE', *, *, #4924, .F. ) ;
#2567 = ORIENTED_EDGE ( 'NONE', *, *, #5259, .T. ) ;
#2568 = AXIS2_PLACEMENT_3D ( 'NONE', #1139, #2845, #2814 ) ;
#2569 = ORIENTED_EDGE ( 'NONE', *, *, #5103, .F. ) ;
#2570 = DIRECTION ( 'NONE',  ( 0.000000000000000000, 0.000000000000000000, -1.000000000000000000 ) ) ;
#2571 = CARTESIAN_POINT ( 'NONE',  ( -311.1905691331858179, 2.276824562219544323E-15, 41.38342604719807127 ) ) ;
#2572 = DIRECTION ( 'NONE',  ( 5.551115123125772841E-17, -1.848892746611743135E-31, -1.000000000000000000 ) ) ;
#2573 = AXIS2_PLACEMENT_3D ( 'NONE', #4392, #1497, #3165 ) ;
#2574 = AXIS2_PLACEMENT_3D ( 'NONE', #690, #1049, #2432 ) ;
#2575 = ORIENTED_EDGE ( 'NONE', *, *, #4366, .F. ) ;
#2576 = CIRCLE ( 'NONE', #2053, 12.50000000000003197 ) ;
#2577 = CARTESIAN_POINT ( 'NONE',  ( -13.17877320795226659, 1.897353801849669836E-15, 47.33401081801162746 ) ) ;
#2578 = EDGE_CURVE ( 'NONE', #3236, #3490, #2536, .T. ) ;
#2579=STYLED_ITEM('',(#5479),#3126);
#2580 = CARTESIAN_POINT ( 'NONE',  ( 0.07030049708446614587, -25.00000000000000355, 219.5055207296742026 ) ) ;
#2581 = CARTESIAN_POINT ( 'NONE',  ( -344.1351952944073105, 5.421010862427522170E-17, 98.54415422078299969 ) ) ;
#2582 = EDGE_CURVE ( 'NONE', #534, #4953, #3854, .T. ) ;
#2583 = EDGE_CURVE ( 'NONE', #2126, #4277, #1511, .T. ) ;
#2584 = VECTOR ( 'NONE', #3513, 1000.000000000000000 ) ;
#2585 = EDGE_CURVE ( 'NONE', #4718, #4330, #4676, .T. ) ;
#2586 = CIRCLE ( 'NONE', #3904, 6.000000000000032863 ) ;
#2587 = VERTEX_POINT ( 'NONE', #442 ) ;
#2588 = ORIENTED_EDGE ( 'NONE', *, *, #1439, .F. ) ;
#2589 = CARTESIAN_POINT ( 'NONE',  ( -0.8482259245422840710, 2.276824562219559311E-15, 36.14439046289818691 ) ) ;
#2590 = CIRCLE ( 'NONE', #4177, 77.49999999999998579 ) ;
#2591 = FACE_OUTER_BOUND ( 'NONE', #2459, .T. ) ;
#2592 = CIRCLE ( 'NONE', #5390, 1.000000000000000888 ) ;
#2593 = ORIENTED_EDGE ( 'NONE', *, *, #85, .T. ) ;
#2594 = CARTESIAN_POINT ( 'NONE',  ( -38.26122282208103798, 0.000000000000000000, 131.6034880481681171 ) ) ;
#2595 = AXIS2_PLACEMENT_3D ( 'NONE', #4899, #4876, #1968 ) ;
#2596 = DIRECTION ( 'NONE',  ( 5.551115123125772841E-17, -1.848892746611743354E-31, -1.000000000000000000 ) ) ;
#2597 = AXIS2_PLACEMENT_3D ( 'NONE', #1480, #3141, #3198 ) ;
#2598 = CARTESIAN_POINT ( 'NONE',  ( -167.9289969670494997, 3.740497495074990297E-15, 528.5729890193238134 ) ) ;
#2599 = CARTESIAN_POINT ( 'NONE',  ( -19.78983854945498422, 2.222614453595284090E-15, 515.1268587725810448 ) ) ;
#2600 = LINE ( 'NONE', #1795, #4861 ) ;
#2601 = ADVANCED_FACE ( 'NONE', ( #967 ), #2560, .T. ) ;
#2602 = ORIENTED_EDGE ( 'NONE', *, *, #1336, .F. ) ;
#2603 = ORIENTED_EDGE ( 'NONE', *, *, #644, .T. ) ;
#2604 = ADVANCED_FACE ( 'NONE', ( #3399, #3917 ), #86, .T. ) ;
#2605 = ORIENTED_EDGE ( 'NONE', *, *, #3499, .F. ) ;
#2606 = CARTESIAN_POINT ( 'NONE',  ( -348.7799179161582970, 14.95948628165116823, 101.1196613272007738 ) ) ;
#2607 = DIRECTION ( 'NONE',  ( 5.551115123125772841E-17, -1.848892746611743135E-31, -1.000000000000000000 ) ) ;
#2608 = ADVANCED_FACE ( 'NONE', ( #915 ), #1268, .T. ) ;
#2609 = CARTESIAN_POINT ( 'NONE',  ( -80.02857808274410445, -21.54565493204321669, -9.999999999999953815 ) ) ;
#2610 = FACE_OUTER_BOUND ( 'NONE', #3732, .T. ) ;
#2611 = ORIENTED_EDGE ( 'NONE', *, *, #823, .F. ) ;
#2612 = CARTESIAN_POINT ( 'NONE',  ( -80.02857808274410445, -21.54565493204320248, -12.00000000000001066 ) ) ;
#2613 = CARTESIAN_POINT ( 'NONE',  ( 8.821273309647297722, 3.740497495074990297E-15, 380.5076279642372015 ) ) ;
#2614 = CARTESIAN_POINT ( 'NONE',  ( 135.7157751673380801, 75.50260479418143689, -10.00000000000006395 ) ) ;
#2615 = APPLICATION_CONTEXT ( 'automotive_design' ) ;
#2616 = EDGE_CURVE ( 'NONE', #3848, #1151, #3039, .T. ) ;
#2617 = ORIENTED_EDGE ( 'NONE', *, *, #2419, .T. ) ;
#2618 = ORIENTED_EDGE ( 'NONE', *, *, #983, .T. ) ;
#2619 = CARTESIAN_POINT ( 'NONE',  ( -74.77857808274400497, 80.45434506795689344, -2.000000000000112355 ) ) ;
#2620 = ADVANCED_FACE ( 'NONE', ( #4735 ), #1792, .T. ) ;
#2621 = ORIENTED_EDGE ( 'NONE', *, *, #2200, .F. ) ;
#2622 = CARTESIAN_POINT ( 'NONE',  ( -57.28677601057280100, 3.252606517456513302E-16, 546.4981013186296650 ) ) ;
#2623 = DIRECTION ( 'NONE',  ( -0.000000000000000000, -1.000000000000000000, -0.000000000000000000 ) ) ;
#2624 = CARTESIAN_POINT ( 'NONE',  ( -330.1866567701584927, 3.740497495074990297E-15, 374.2973685668102917 ) ) ;
#2625 = CARTESIAN_POINT ( 'NONE',  ( -264.1404626571534777, 2.222614453595284090E-15, 511.7445549721628595 ) ) ;
#2626 = DIRECTION ( 'NONE',  ( -0.9998833722232041143, 6.892903270961872452E-31, 0.01527226085271972227 ) ) ;
#2627 = VERTEX_POINT ( 'NONE', #4300 ) ;
#2628 = ORIENTED_EDGE ( 'NONE', *, *, #1854, .T. ) ;
#2629 = ORIENTED_EDGE ( 'NONE', *, *, #796, .T. ) ;
#2630 = DIRECTION ( 'NONE',  ( 0.000000000000000000, 0.000000000000000000, 1.000000000000000000 ) ) ;
#2631 = DIRECTION ( 'NONE',  ( 0.09383933793885568253, -2.673190762809473730E-31, -0.9955873536034882676 ) ) ;
#2632 = CYLINDRICAL_SURFACE ( 'NONE', #4943, 6.000000000000032863 ) ;
#2633 = FILL_AREA_STYLE_COLOUR ( '', #1434 ) ;
#2634 = EDGE_LOOP ( 'NONE', ( #2232, #2657, #1711, #2335 ) ) ;
#2635 = DIRECTION ( 'NONE',  ( 1.000000000000000000, -3.851859888774468203E-31, 0.000000000000000000 ) ) ;
#2636 = CARTESIAN_POINT ( 'NONE',  ( -320.6447527397745034, -25.00000000000003197, 453.8399743637903612 ) ) ;
#2637 = CARTESIAN_POINT ( 'NONE',  ( -365.8191009029663974, 5.636683259291067391E-15, 36.23439996194949941 ) ) ;
#2638 = ORIENTED_EDGE ( 'NONE', *, *, #765, .F. ) ;
#2639 = DIRECTION ( 'NONE',  ( 0.9998833722232040033, -6.797399803719615819E-31, -0.01527226085271964420 ) ) ;
#2640 = ORIENTED_EDGE ( 'NONE', *, *, #5068, .T. ) ;
#2641 = CARTESIAN_POINT ( 'NONE',  ( 35.78913469918423829, 0.000000000000000000, 310.6402212931345161 ) ) ;
#2642 = VERTEX_POINT ( 'NONE', #3792 ) ;
#2643 = DIRECTION ( 'NONE',  ( -0.9955873536034882676, 5.453577263127812432E-31, -0.09383933793885552987 ) ) ;
#2644 = CARTESIAN_POINT ( 'NONE',  ( -342.0170653153606395, 3.740497495074990297E-15, 268.9367132353195302 ) ) ;
#2645 = CARTESIAN_POINT ( 'NONE',  ( 18.31346110193232590, 2.222614453595284090E-15, 444.2932575970293101 ) ) ;
#2646 = LINE ( 'NONE', #555, #4690 ) ;
#2647 = EDGE_CURVE ( 'NONE', #4331, #4307, #4244, .T. ) ;
#2648 = EDGE_CURVE ( 'NONE', #3875, #2651, #549, .T. ) ;
#2649 = ORIENTED_EDGE ( 'NONE', *, *, #56, .T. ) ;
#2650 = VERTEX_POINT ( 'NONE', #3878 ) ;
#2651 = VERTEX_POINT ( 'NONE', #2118 ) ;
#2652 = CIRCLE ( 'NONE', #1595, 50.00000000000000000 ) ;
#2653 = DIRECTION ( 'NONE',  ( -5.679099018122554920E-31, -1.000000000000000000, 2.149753974990777610E-31 ) ) ;
#2654 = DIRECTION ( 'NONE',  ( -0.9955873536034882676, 5.502656983963321189E-31, -0.09383933793885573804 ) ) ;
#2655 = CARTESIAN_POINT ( 'NONE',  ( 151.9714219172562935, -25.54565493204309234, -5.551115123125782702E-14 ) ) ;
#2656 = CARTESIAN_POINT ( 'NONE',  ( 137.9714219172562082, 98.45434506795683660, 152.0000000000003126 ) ) ;
#2657 = ORIENTED_EDGE ( 'NONE', *, *, #4855, .T. ) ;
#2658 = FACE_OUTER_BOUND ( 'NONE', #611, .T. ) ;
#2659 = CARTESIAN_POINT ( 'NONE',  ( 36.66581985038869362, 3.252606517456513302E-16, 340.1662229844753256 ) ) ;
#2660 = CARTESIAN_POINT ( 'NONE',  ( -338.5048350180761076, 2.276824562219559311E-15, 38.80891300457378890 ) ) ;
#2661 = CIRCLE ( 'NONE', #2837, 5.250000000000004441 ) ;
#2662 = AXIS2_PLACEMENT_3D ( 'NONE', #4949, #3315, #745 ) ;
#2663 = ORIENTED_EDGE ( 'NONE', *, *, #335, .F. ) ;
#2664 = CARTESIAN_POINT ( 'NONE',  ( -14.89480152442229688, 0.000000000000000000, 508.6517828409968729 ) ) ;
#2665 = DIRECTION ( 'NONE',  ( 0.9444589563252840936, 1.395212689362338787E-17, -0.3286293958503336277 ) ) ;
#2666 = CIRCLE ( 'NONE', #207, 6.000000000000032863 ) ;
#2667 = AXIS2_PLACEMENT_3D ( 'NONE', #1086, #4903, #1116 ) ;
#2668 = VERTEX_POINT ( 'NONE', #2183 ) ;
#2669 = CARTESIAN_POINT ( 'NONE',  ( -364.1439395362591540, 2.222614453595284090E-15, 237.2787335496894343 ) ) ;
#2670 = VERTEX_POINT ( 'NONE', #3831 ) ;
#2671 = CIRCLE ( 'NONE', #4082, 40.00000000000000000 ) ;
#2672 = AXIS2_PLACEMENT_3D ( 'NONE', #4700, #101, #1779 ) ;
#2673 = LINE ( 'NONE', #3587, #21 ) ;
#2674 = CIRCLE ( 'NONE', #3997, 4.382543221487789964 ) ;
#2675 = CARTESIAN_POINT ( 'NONE',  ( -349.8593949086763928, 2.222614453595284090E-15, 159.2749827905956010 ) ) ;
#2676 = FACE_OUTER_BOUND ( 'NONE', #3589, .T. ) ;
#2677 = CIRCLE ( 'NONE', #3910, 5.250000000000004441 ) ;
#2678 = ORIENTED_EDGE ( 'NONE', *, *, #2208, .T. ) ;
#2679 = EDGE_CURVE ( 'NONE', #2642, #864, #3483, .T. ) ;
#2680 = EDGE_LOOP ( 'NONE', ( #2531, #4362, #2867, #3010 ) ) ;
#2681 = DIRECTION ( 'NONE',  ( 0.09383933793885568253, -2.673190762809473730E-31, -0.9955873536034882676 ) ) ;
#2682 = EDGE_CURVE ( 'NONE', #5397, #486, #4272, .T. ) ;
#2683 = CARTESIAN_POINT ( 'NONE',  ( -345.9181427152443007, 2.222614453595284090E-15, 117.4603139392499429 ) ) ;
#2684 = DIRECTION ( 'NONE',  ( -1.000000000000000000, 3.759415251443877379E-31, -5.551115123125772841E-17 ) ) ;
#2685 = EDGE_CURVE ( 'NONE', #3281, #2521, #4763, .T. ) ;
#2686 =( NAMED_UNIT ( * ) PLANE_ANGLE_UNIT ( ) SI_UNIT ( $, .RADIAN. ) );
#2687 = VERTEX_POINT ( 'NONE', #3063 ) ;
#2688 = DIRECTION ( 'NONE',  ( 1.000000000000000000, -3.759415251443877379E-31, 5.551115123125772841E-17 ) ) ;
#2689 = CARTESIAN_POINT ( 'NONE',  ( 36.35777514575907787, -24.99999999999981881, 354.7349908125917750 ) ) ;
#2690 = DIRECTION ( 'NONE',  ( 0.9955873536034882676, 0.000000000000000000, 0.09383933793885600172 ) ) ;
#2691 = DIRECTION ( 'NONE',  ( 5.551115123125772841E-17, -1.848892746611743135E-31, -1.000000000000000000 ) ) ;
#2692 = CIRCLE ( 'NONE', #3929, 22.67218956682437536 ) ;
#2693 = DIRECTION ( 'NONE',  ( 1.000000000000000000, 0.000000000000000000, 8.260587980841931384E-17 ) ) ;
#2694 = CARTESIAN_POINT ( 'NONE',  ( -156.9923520473269321, 0.000000000000000000, 556.8176423728721147 ) ) ;
#2695 = VERTEX_POINT ( 'NONE', #553 ) ;
#2696 = CARTESIAN_POINT ( 'NONE',  ( 31.14585677005056041, 25.00000000000018474, 398.7793066466517757 ) ) ;
#2697 = ORIENTED_EDGE ( 'NONE', *, *, #1284, .T. ) ;
#2698 = VECTOR ( 'NONE', #3053, 1000.000000000000114 ) ;
#2699 = DIRECTION ( 'NONE',  ( -5.551115123125772841E-17, 1.848892746611743135E-31, 1.000000000000000000 ) ) ;
#2700 = LINE ( 'NONE', #4379, #2312 ) ;
#2701 = VECTOR ( 'NONE', #597, 1000.000000000000227 ) ;
#2702 = ORIENTED_EDGE ( 'NONE', *, *, #4994, .T. ) ;
#2703 = ORIENTED_EDGE ( 'NONE', *, *, #617, .T. ) ;
#2704 = ADVANCED_FACE ( 'NONE', ( #142 ), #1818, .F. ) ;
#2705 = CARTESIAN_POINT ( 'NONE',  ( -311.1905691331858179, 2.276824562219544323E-15, 41.38342604719806417 ) ) ;
#2706 = CIRCLE ( 'NONE', #2092, 56.63911695420812009 ) ;
#2707 = DIRECTION ( 'NONE',  ( -5.679099018122554920E-31, -1.000000000000000000, 2.149753974990777610E-31 ) ) ;
#2708 = CARTESIAN_POINT ( 'NONE',  ( -13.17877320795226659, 1.897353801849669836E-15, 47.33401081801162746 ) ) ;
#2709 = CARTESIAN_POINT ( 'NONE',  ( -342.9618789639491752, 2.813531315051557923E-15, 39.39324540378412109 ) ) ;
#2710 = ORIENTED_EDGE ( 'NONE', *, *, #3288, .F. ) ;
#2711 = DIRECTION ( 'NONE',  ( -5.551115123125772841E-17, 1.848892746611743354E-31, 1.000000000000000000 ) ) ;
#2712 = CARTESIAN_POINT ( 'NONE',  ( -360.7307227603797060, -24.99999999999981881, 354.4373729494859049 ) ) ;
#2713 = DIRECTION ( 'NONE',  ( 0.09383933793885568253, -2.673190762809473730E-31, -0.9955873536034882676 ) ) ;
#2714 = LINE ( 'NONE', #2771, #2048 ) ;
#2715 = DIRECTION ( 'NONE',  ( -0.9955873536034883786, 5.430490990731020552E-31, -0.09383933793885548824 ) ) ;
#2716 = CARTESIAN_POINT ( 'NONE',  ( -1.533280346156490337, 2.222614453595284090E-15, 488.4857301958385278 ) ) ;
#2717 = ORIENTED_EDGE ( 'NONE', *, *, #894, .T. ) ;
#2718 = CARTESIAN_POINT ( 'NONE',  ( -122.4270646331732451, 25.00000000000018474, 560.5113017241552598 ) ) ;
#2719 = ORIENTED_EDGE ( 'NONE', *, *, #560, .F. ) ;
#2720 = DIRECTION ( 'NONE',  ( 0.000000000000000000, -1.000000000000000000, 0.000000000000000000 ) ) ;
#2721 = DIRECTION ( 'NONE',  ( -1.000000000000000000, -1.219242865862094703E-16, 0.000000000000000000 ) ) ;
#2722 = VERTEX_POINT ( 'NONE', #2338 ) ;
#2723 = EDGE_LOOP ( 'NONE', ( #4375, #3418, #5247, #2410, #387, #2213, #3178, #1780 ) ) ;
#2724 = CARTESIAN_POINT ( 'NONE',  ( -351.7361816674535362, 5.421010862427522170E-17, 179.1867298626658283 ) ) ;
#2725 = DIRECTION ( 'NONE',  ( 0.000000000000000000, 1.000000000000000000, 0.000000000000000000 ) ) ;
#2726 = DIRECTION ( 'NONE',  ( 0.000000000000000000, 1.000000000000000000, 0.000000000000000000 ) ) ;
#2727 = DIRECTION ( 'NONE',  ( 0.000000000000000000, -0.000000000000000000, 1.000000000000000000 ) ) ;
#2728 = EDGE_LOOP ( 'NONE', ( #2955, #3125 ) ) ;
#2729 = FILL_AREA_STYLE ('',( #1171 ) ) ;
#2730 = CARTESIAN_POINT ( 'NONE',  ( -359.3101886666408404, 0.000000000000000000, 100.1271279930180356 ) ) ;
#2731 = CARTESIAN_POINT ( 'NONE',  ( -14.89480152442222582, -24.99999999999981881, 508.6517828409982940 ) ) ;
#2732 = CARTESIAN_POINT ( 'NONE',  ( -51.80562710762752232, 0.000000000000000000, 127.0899108387844336 ) ) ;
#2733 = TOROIDAL_SURFACE ( 'NONE', #4585, 30.50000000000110845, 1.000000000000000000 ) ;
#2734 = DIRECTION ( 'NONE',  ( 5.551115123125772841E-17, -1.848892746611743135E-31, -1.000000000000000000 ) ) ;
#2735 = EDGE_CURVE ( 'NONE', #2587, #2803, #5166, .T. ) ;
#2736 = CIRCLE ( 'NONE', #1508, 5.250000000000018652 ) ;
#2737 = EDGE_CURVE ( 'NONE', #2162, #2116, #3545, .T. ) ;
#2738 = CARTESIAN_POINT ( 'NONE',  ( -323.1742634138752805, 5.712857831165392007E-15, 179.8699762867167351 ) ) ;
#2739 = CARTESIAN_POINT ( 'NONE',  ( 16.26935751051938439, 25.00000000000000355, 140.3055424402287770 ) ) ;
#2740 = APPLICATION_PROTOCOL_DEFINITION ( 'draft international standard', 'automotive_design', 1998, #1756 ) ;
#2741 = CARTESIAN_POINT ( 'NONE',  ( -299.8611223228771792, -25.00000000000003197, 439.6443911606498887 ) ) ;
#2742 = EDGE_CURVE ( 'NONE', #5300, #2427, #5017, .T. ) ;
#2743 = ADVANCED_FACE ( 'NONE', ( #2282 ), #192, .T. ) ;
#2744 = VECTOR ( 'NONE', #306, 1000.000000000000114 ) ;
#2745 = EDGE_LOOP ( 'NONE', ( #5059, #1545, #1224, #417, #1739, #2484, #5354, #1274 ) ) ;
#2746 = CARTESIAN_POINT ( 'NONE',  ( -16.96312831416361533, 25.00000000000018474, 463.2830513152442222 ) ) ;
#2747 = ORIENTED_EDGE ( 'NONE', *, *, #2182, .F. ) ;
#2748 = ADVANCED_FACE ( 'NONE', ( #1045 ), #995, .F. ) ;
#2749 = FACE_OUTER_BOUND ( 'NONE', #552, .T. ) ;
#2750 = CIRCLE ( 'NONE', #3124, 21.00000000000012790 ) ;
#2751=STYLED_ITEM('',(#5458),#3192);
#2752 = PLANE ( 'NONE',  #1257 ) ;
#2753 = COLOUR_RGB ( '',0.7921568627450980005, 0.8196078431372548767, 0.9333333333333333481 ) ;
#2754 = ORIENTED_EDGE ( 'NONE', *, *, #720, .F. ) ;
#2755 = AXIS2_PLACEMENT_3D ( 'NONE', #2581, #1339, #4992 ) ;
#2756 = VERTEX_POINT ( 'NONE', #1021 ) ;
#2757 = CARTESIAN_POINT ( 'NONE',  ( -84.02857808274400497, -39.54565493204319182, -5.551115123125782702E-14 ) ) ;
#2758 = FACE_BOUND ( 'NONE', #3750, .T. ) ;
#2759 = CARTESIAN_POINT ( 'NONE',  ( 113.4038502097781276, 15.00000000000001421, 172.0544138201894668 ) ) ;
#2760 = FACE_OUTER_BOUND ( 'NONE', #2558, .T. ) ;
#2761 = AXIS2_PLACEMENT_3D ( 'NONE', #135, #4727, #3577 ) ;
#2762 = AXIS2_PLACEMENT_3D ( 'NONE', #2433, #3619, #717 ) ;
#2763 = CARTESIAN_POINT ( 'NONE',  ( -77.50517668553013095, 0.000000000000000000, 131.6034880481681171 ) ) ;
#2764 = ORIENTED_EDGE ( 'NONE', *, *, #226, .T. ) ;
#2765 = EDGE_CURVE ( 'NONE', #689, #4644, #5194, .T. ) ;
#2766 = SURFACE_SIDE_STYLE ('',( #2291 ) ) ;
#2767 = DIRECTION ( 'NONE',  ( 1.000000000000000000, -3.759415251443877817E-31, 5.551115123125772841E-17 ) ) ;
#2768 = DIRECTION ( 'NONE',  ( 0.000000000000000000, -1.000000000000000000, 0.000000000000000000 ) ) ;
#2769 = PLANE ( 'NONE',  #1267 ) ;
#2770 = AXIS2_PLACEMENT_3D ( 'NONE', #3111, #1095, #5239 ) ;
#2771 = CARTESIAN_POINT ( 'NONE',  ( -84.02857808274397655, -39.54565493204319893, 152.0000000000000853 ) ) ;
#2772 = CARTESIAN_POINT ( 'NONE',  ( 11.81831109762776322, 2.276824562219553001E-15, 46.95220429669362971 ) ) ;
#2773 = CARTESIAN_POINT ( 'NONE',  ( 9.699276322990401766, 25.00000000000018474, 297.8714164406044915 ) ) ;
#2774 = EDGE_CURVE ( 'NONE', #2687, #1665, #3121, .T. ) ;
#2775 = CARTESIAN_POINT ( 'NONE',  ( -1.533280346156948193, -24.99999999999981881, 488.4857301958397784 ) ) ;
#2776 = DIRECTION ( 'NONE',  ( 1.000000000000000000, 0.000000000000000000, 7.228014483236656373E-17 ) ) ;
#2777 = EDGE_CURVE ( 'NONE', #1327, #405, #2673, .T. ) ;
#2778 = ORIENTED_EDGE ( 'NONE', *, *, #5123, .F. ) ;
#2779 = CARTESIAN_POINT ( 'NONE',  ( -167.9289969670495282, 25.00000000000018474, 528.5729890193230176 ) ) ;
#2780 = VERTEX_POINT ( 'NONE', #1926 ) ;
#2781 = DIRECTION ( 'NONE',  ( 0.000000000000000000, 1.000000000000000000, 0.000000000000000000 ) ) ;
#2782 = DIRECTION ( 'NONE',  ( -0.09383933793885536334, 2.626968444144180070E-31, 0.9955873536034882676 ) ) ;
#2783 =( REPRESENTATION_RELATIONSHIP ('NONE','NONE', #2124, #2334 ) REPRESENTATION_RELATIONSHIP_WITH_TRANSFORMATION ( #5380 )SHAPE_REPRESENTATION_RELATIONSHIP( ) );
#2784 = ORIENTED_EDGE ( 'NONE', *, *, #4460, .F. ) ;
#2785 = CIRCLE ( 'NONE', #4547, 4.382543221487789076 ) ;
#2786 = ORIENTED_EDGE ( 'NONE', *, *, #4793, .F. ) ;
#2787 = DIRECTION ( 'NONE',  ( 5.551115123125772841E-17, -1.848892746611743135E-31, -1.000000000000000000 ) ) ;
#2788 = CARTESIAN_POINT ( 'NONE',  ( 96.73877717791896202, -14.99999999999998579, 67.09613410133256650 ) ) ;
#2789 = CARTESIAN_POINT ( 'NONE',  ( -344.4167133082243595, 2.222614453595284090E-15, 101.5309162815936048 ) ) ;
#2790 = DIRECTION ( 'NONE',  ( -5.551115123125772841E-17, 1.848892746611743135E-31, 1.000000000000000000 ) ) ;
#2791 = ORIENTED_EDGE ( 'NONE', *, *, #2339, .T. ) ;
#2792 = AXIS2_PLACEMENT_3D ( 'NONE', #5181, #1016, #185 ) ;
#2793 = CARTESIAN_POINT ( 'NONE',  ( 136.6230329513292361, -17.01448963777488288, -9.999999999999953815 ) ) ;
#2794 = DIRECTION ( 'NONE',  ( -0.09383933793885537722, 2.626968444144180508E-31, 0.9955873536034883786 ) ) ;
#2795 = DIRECTION ( 'NONE',  ( 0.09383933793885537722, -2.626968444144180508E-31, -0.9955873536034883786 ) ) ;
#2796 = DIRECTION ( 'NONE',  ( -5.551115123125772841E-17, 1.848892746611743354E-31, 1.000000000000000000 ) ) ;
#2797 = PLANE ( 'NONE',  #1426 ) ;
#2798 = CARTESIAN_POINT ( 'NONE',  ( -338.5986743560152377, 2.276824562219559311E-15, 39.80450035817695209 ) ) ;
#2799 = CARTESIAN_POINT ( 'NONE',  ( -86.97194166595193110, 25.00000000000018474, 531.0655262460722952 ) ) ;
#2800 = CARTESIAN_POINT ( 'NONE',  ( 18.31346110193232590, 2.222614453595284090E-15, 444.2932575970293101 ) ) ;
#2801 = CARTESIAN_POINT ( 'NONE',  ( 137.9714219172561513, 98.45434506795689344, -12.00000000000006573 ) ) ;
#2802 = CIRCLE ( 'NONE', #1402, 12.50000000000003197 ) ;
#2803 = VERTEX_POINT ( 'NONE', #603 ) ;
#2804 = CARTESIAN_POINT ( 'NONE',  ( -334.2906958041451162, 24.99999999999997158, 430.9840019716597226 ) ) ;
#2805 = EDGE_LOOP ( 'NONE', ( #2618, #350, #2990, #5165 ) ) ;
#2806 = DIRECTION ( 'NONE',  ( -5.551115123125772841E-17, 1.848892746611743135E-31, 1.000000000000000000 ) ) ;
#2807 = DIRECTION ( 'NONE',  ( 5.551115123125772841E-17, -1.848892746611743135E-31, -1.000000000000000000 ) ) ;
#2808 = ORIENTED_EDGE ( 'NONE', *, *, #3718, .F. ) ;
#2809 = UNCERTAINTY_MEASURE_WITH_UNIT (LENGTH_MEASURE( 1.000000000000000082E-05 ), #988, 'distance_accuracy_value', 'NONE');
#2810 = ORIENTED_EDGE ( 'NONE', *, *, #2816, .F. ) ;
#2811 = DIRECTION ( 'NONE',  ( 0.01527226085271972227, 2.095411779493299033E-31, 0.9998833722232041143 ) ) ;
#2812 = DIRECTION ( 'NONE',  ( 0.000000000000000000, 0.000000000000000000, 1.000000000000000000 ) ) ;
#2813 = EDGE_CURVE ( 'NONE', #4708, #3749, #2661, .T. ) ;
#2814 = DIRECTION ( 'NONE',  ( -0.9955873536034884896, 5.465719896581968711E-31, -0.09383933793885443353 ) ) ;
#2815 = DIRECTION ( 'NONE',  ( 5.551115123125772841E-17, -1.848892746611743135E-31, -1.000000000000000000 ) ) ;
#2816 = EDGE_CURVE ( 'NONE', #1728, #4985, #4678, .T. ) ;
#2817 = APPLICATION_CONTEXT ( 'automotive_design' ) ;
#2818 = EDGE_CURVE ( 'NONE', #5060, #5244, #3558, .T. ) ;
#2819 = DIRECTION ( 'NONE',  ( 0.09383933793885568253, -2.673190762809473730E-31, -0.9955873536034882676 ) ) ;
#2820 = ORIENTED_EDGE ( 'NONE', *, *, #1266, .T. ) ;
#2821 =( LENGTH_UNIT ( ) NAMED_UNIT ( * ) SI_UNIT ( .MILLI., .METRE. ) );
#2822 = FACE_OUTER_BOUND ( 'NONE', #2680, .T. ) ;
#2823 = CARTESIAN_POINT ( 'NONE',  ( -122.4270646331731598, 3.252606517456513302E-16, 560.5113017241549187 ) ) ;
#2824 = CARTESIAN_POINT ( 'NONE',  ( -318.3107145942876173, 2.222614453595271862E-15, 160.2397472284629885 ) ) ;
#2825 = FACE_OUTER_BOUND ( 'NONE', #2723, .T. ) ;
#2826 = CARTESIAN_POINT ( 'NONE',  ( -72.60637664584220374, 25.00000000000018474, 552.9197695054134556 ) ) ;
#2827 = SHAPE_DEFINITION_REPRESENTATION ( #4520, #3052 ) ;
#2828 = CARTESIAN_POINT ( 'NONE',  ( -105.2090356704105147, 2.222614453595284090E-15, 560.1816718768288865 ) ) ;
#2829 = AXIS2_PLACEMENT_3D ( 'NONE', #4223, #3409, #3015 ) ;
#2830 = ORIENTED_EDGE ( 'NONE', *, *, #2105, .T. ) ;
#2831 = CARTESIAN_POINT ( 'NONE',  ( -23.53079058812344471, 25.00000000000018474, 476.4235034963351154 ) ) ;
#2832 = ORIENTED_EDGE ( 'NONE', *, *, #1083, .T. ) ;
#2833 = AXIS2_PLACEMENT_3D ( 'NONE', #4627, #3428, #1671 ) ;
#2834 = ADVANCED_FACE ( 'NONE', ( #3964 ), #4456, .T. ) ;
#2835 = CARTESIAN_POINT ( 'NONE',  ( 131.3198108831832087, -26.07682022631159668, -10.00000000000000888 ) ) ;
#2836 =( NAMED_UNIT ( * ) SI_UNIT ( $, .STERADIAN. ) SOLID_ANGLE_UNIT ( ) );
#2837 = AXIS2_PLACEMENT_3D ( 'NONE', #4353, #2258, #580 ) ;
#2838 = CIRCLE ( 'NONE', #3368, 5.250000000000018652 ) ;
#2839 = ORIENTED_EDGE ( 'NONE', *, *, #2914, .T. ) ;
#2840 = AXIS2_PLACEMENT_3D ( 'NONE', #66, #1631, #3347 ) ;
#2841 = CIRCLE ( 'NONE', #641, 5.250000000000018652 ) ;
#2842 = EDGE_LOOP ( 'NONE', ( #3584, #2900, #4842, #1319 ) ) ;
#2843 = DIRECTION ( 'NONE',  ( -0.9955873536034882676, 5.436595176548168253E-31, -0.09383933793885512742 ) ) ;
#2844 = FACE_BOUND ( 'NONE', #3567, .T. ) ;
#2845 = DIRECTION ( 'NONE',  ( 0.09383933793885568253, -2.673190762809473730E-31, -0.9955873536034882676 ) ) ;
#2846 = DIRECTION ( 'NONE',  ( -1.000000000000000000, 0.000000000000000000, -8.260587980841931384E-17 ) ) ;
#2847 = VECTOR ( 'NONE', #2807, 1000.000000000000000 ) ;
#2848 = ADVANCED_FACE ( 'NONE', ( #2749 ), #686, .F. ) ;
#2849 = AXIS2_PLACEMENT_3D ( 'NONE', #4233, #3819, #495 ) ;
#2850 = CARTESIAN_POINT ( 'NONE',  ( 139.2214219172562650, -21.54565493204319182, -26.84924240491753977 ) ) ;
#2851 = ORIENTED_EDGE ( 'NONE', *, *, #5257, .T. ) ;
#2852 = EDGE_CURVE ( 'NONE', #5244, #4403, #1682, .T. ) ;
#2853 = CARTESIAN_POINT ( 'NONE',  ( 137.9714219172561513, 98.45434506795687923, -12.00000000000006573 ) ) ;
#2854 = EDGE_CURVE ( 'NONE', #4218, #2780, #812, .T. ) ;
#2855 = AXIS2_PLACEMENT_3D ( 'NONE', #730, #4933, #3684 ) ;
#2856 = CARTESIAN_POINT ( 'NONE',  ( -174.3534642324304116, 5.421010862427522170E-17, 552.7876087698471110 ) ) ;
#2857 = FACE_BOUND ( 'NONE', #757, .T. ) ;
#2858 = VECTOR ( 'NONE', #3758, 1000.000000000000114 ) ;
#2859 = CIRCLE ( 'NONE', #4345, 30.50000000000124345 ) ;
#2860 = DIRECTION ( 'NONE',  ( 5.551115123125772841E-17, -1.848892746611743135E-31, -1.000000000000000000 ) ) ;
#2861 = CIRCLE ( 'NONE', #4419, 12.50000000000003197 ) ;
#2862 = DIRECTION ( 'NONE',  ( -5.720779902258401340E-31, -1.000000000000000000, 2.099398147291833041E-31 ) ) ;
#2863 = CARTESIAN_POINT ( 'NONE',  ( -152.2642418385221674, 25.00000000000018474, 532.1805559224801527 ) ) ;
#2864 = CARTESIAN_POINT ( 'NONE',  ( -264.1404626571534777, 2.222614453595284090E-15, 511.7445549721628595 ) ) ;
#2865 = ORIENTED_EDGE ( 'NONE', *, *, #2765, .F. ) ;
#2866 = CARTESIAN_POINT ( 'NONE',  ( -23.53079058812296154, 3.740497495074990297E-15, 476.4235034963361954 ) ) ;
#2867 = ORIENTED_EDGE ( 'NONE', *, *, #4133, .F. ) ;
#2868 = DIRECTION ( 'NONE',  ( -1.000000000000000000, 0.000000000000000000, 0.000000000000000000 ) ) ;
#2869 = CARTESIAN_POINT ( 'NONE',  ( -84.02857808274407603, 84.45434506795682239, -11.99999999999995559 ) ) ;
#2870 = ORIENTED_EDGE ( 'NONE', *, *, #228, .F. ) ;
#2871 = EDGE_LOOP ( 'NONE', ( #2050, #221, #2588, #1314, #4510, #841, #5336, #520 ) ) ;
#2872 = DIRECTION ( 'NONE',  ( -1.000000000000000000, 0.000000000000000000, 0.000000000000000000 ) ) ;
#2873 = CARTESIAN_POINT ( 'NONE',  ( -353.5191290882918338, 0.000000000000000000, 198.1028895811323025 ) ) ;
#2874 = CARTESIAN_POINT ( 'NONE',  ( -84.02857808274397655, -39.54565493204319893, 152.0000000000000853 ) ) ;
#2875 = CARTESIAN_POINT ( 'NONE',  ( -80.02857808274401918, 80.45434506795689344, -12.00000000000001066 ) ) ;
#2876 = DIRECTION ( 'NONE',  ( 0.000000000000000000, 0.000000000000000000, 1.000000000000000000 ) ) ;
#2877 = VERTEX_POINT ( 'NONE', #279 ) ;
#2878 = EDGE_CURVE ( 'NONE', #3515, #3229, #3173, .T. ) ;
#2879 = ORIENTED_EDGE ( 'NONE', *, *, #4701, .T. ) ;
#2880 = DIRECTION ( 'NONE',  ( -5.551115123125772841E-17, 1.848892746611743135E-31, 1.000000000000000000 ) ) ;
#2881 = AXIS2_PLACEMENT_3D ( 'NONE', #5258, #2794, #5318 ) ;
#2882 = CARTESIAN_POINT ( 'NONE',  ( -367.0460729392618759, 0.000000000000000000, 268.0688838304710089 ) ) ;
#2883 = CARTESIAN_POINT ( 'NONE',  ( -347.8887688119603467, 2.222614453595284090E-15, 138.3676483649222178 ) ) ;
#2884 = PLANE ( 'NONE',  #5202 ) ;
#2885 = FACE_OUTER_BOUND ( 'NONE', #3774, .T. ) ;
#2886 = CARTESIAN_POINT ( 'NONE',  ( -264.1404626571541598, 24.99999999999997158, 511.7445549721641100 ) ) ;
#2887 = CARTESIAN_POINT ( 'NONE',  ( 33.59898979596707136, -24.99999999999981881, 384.0431050523492900 ) ) ;
#2888 = EDGE_CURVE ( 'NONE', #3915, #4297, #3105, .T. ) ;
#2889 = ORIENTED_EDGE ( 'NONE', *, *, #644, .F. ) ;
#2890 = VERTEX_POINT ( 'NONE', #1978 ) ;
#2891 = DIRECTION ( 'NONE',  ( -1.000000000000000000, 0.000000000000000000, 0.000000000000000000 ) ) ;
#2892 = DIRECTION ( 'NONE',  ( 0.000000000000000000, 0.000000000000000000, 1.000000000000000000 ) ) ;
#2893 = ORIENTED_EDGE ( 'NONE', *, *, #3885, .T. ) ;
#2894 = ADVANCED_FACE ( 'NONE', ( #651 ), #1477, .T. ) ;
#2895 = FACE_OUTER_BOUND ( 'NONE', #2492, .T. ) ;
#2896 = DIRECTION ( 'NONE',  ( 0.09383933793885568253, -2.673190762809473730E-31, -0.9955873536034882676 ) ) ;
#2897 = CARTESIAN_POINT ( 'NONE',  ( 133.9714219172562366, 80.45434506795683660, -12.00000000000001066 ) ) ;
#2898 = DIRECTION ( 'NONE',  ( 0.000000000000000000, 0.000000000000000000, -1.000000000000000000 ) ) ;
#2899 = ORIENTED_EDGE ( 'NONE', *, *, #156, .F. ) ;
#2900 = ORIENTED_EDGE ( 'NONE', *, *, #4812, .F. ) ;
#2901 = DIRECTION ( 'NONE',  ( -0.000000000000000000, -1.000000000000000000, -0.000000000000000000 ) ) ;
#2902 = CYLINDRICAL_SURFACE ( 'NONE', #3711, 27.50000000000126121 ) ;
#2903 = LINE ( 'NONE', #5403, #570 ) ;
#2904 = SURFACE_STYLE_FILL_AREA ( #3383 ) ;
#2905 = CARTESIAN_POINT ( 'NONE',  ( -63.04765821499436385, 1.843143693225357538E-15, 521.0401840782876661 ) ) ;
#2906 = CARTESIAN_POINT ( 'NONE',  ( 10.82492224058160879, -24.99999999999981881, 312.2165827548579387 ) ) ;
#2907 = DIRECTION ( 'NONE',  ( 0.9955873536034883786, -5.498529991225532086E-31, 0.09383933793885522456 ) ) ;
#2908 = ADVANCED_FACE ( 'NONE', ( #3194 ), #2797, .F. ) ;
#2909 = ORIENTED_EDGE ( 'NONE', *, *, #5085, .T. ) ;
#2910 = EDGE_CURVE ( 'NONE', #1728, #195, #4476, .T. ) ;
#2911 = CIRCLE ( 'NONE', #1775, 30.50000000000124345 ) ;
#2912 = ADVANCED_FACE ( 'NONE', ( #4013 ), #1059, .T. ) ;
#2913 = LINE ( 'NONE', #4110, #1796 ) ;
#2914 = EDGE_CURVE ( 'NONE', #1142, #8, #2303, .T. ) ;
#2915 = SURFACE_STYLE_USAGE ( .BOTH. , #3694 ) ;
#2916 = AXIS2_PLACEMENT_3D ( 'NONE', #3295, #1994, #1490 ) ;
#2917 = ORIENTED_EDGE ( 'NONE', *, *, #5425, .F. ) ;
#2918 = EDGE_LOOP ( 'NONE', ( #2374, #2371, #1952, #2343 ) ) ;
#2919 = DIRECTION ( 'NONE',  ( 0.09383933793885568253, -2.673190762809473730E-31, -0.9955873536034882676 ) ) ;
#2920 = VECTOR ( 'NONE', #2699, 1000.000000000000000 ) ;
#2921 = DIRECTION ( 'NONE',  ( 0.09383933793885568253, -2.673190762809473730E-31, -0.9955873536034882676 ) ) ;
#2922 = CARTESIAN_POINT ( 'NONE',  ( 29.23877717791899755, 0.000000000000000000, 67.09613410133263756 ) ) ;
#2923 = DIRECTION ( 'NONE',  ( -0.09383933793885537722, 2.626968444144180508E-31, 0.9955873536034883786 ) ) ;
#2924 = VERTEX_POINT ( 'NONE', #2297 ) ;
#2925 = AXIS2_PLACEMENT_3D ( 'NONE', #596, #5427, #1683 ) ;
#2926 = AXIS2_PLACEMENT_3D ( 'NONE', #4646, #959, #1347 ) ;
#2927 = EDGE_LOOP ( 'NONE', ( #3565, #2190, #5177, #1408 ) ) ;
#2928 = LINE ( 'NONE', #1200, #1977 ) ;
#2929 = CARTESIAN_POINT ( 'NONE',  ( 0.000000000000000000, 80.00000000000000000, 0.000000000000000000 ) ) ;
#2930 = CARTESIAN_POINT ( 'NONE',  ( 29.23877717791899755, 0.000000000000000000, 67.09613410133263756 ) ) ;
#2931 = PRESENTATION_LAYER_ASSIGNMENT (  '', '', ( #1521 ) ) ;
#2932 = AXIS2_PLACEMENT_3D ( 'NONE', #4033, #3519, #4817 ) ;
#2933 = EDGE_CURVE ( 'NONE', #405, #3749, #4851, .T. ) ;
#2934 =( LENGTH_UNIT ( ) NAMED_UNIT ( * ) SI_UNIT ( .MILLI., .METRE. ) );
#2935 = AXIS2_PLACEMENT_3D ( 'NONE', #2557, #2480, #3316 ) ;
#2936 = AXIS2_PLACEMENT_3D ( 'NONE', #1523, #1112, #4410 ) ;
#2937 = AXIS2_PLACEMENT_3D ( 'NONE', #4010, #325, #1999 ) ;
#2938 = CARTESIAN_POINT ( 'NONE',  ( -268.5984117390374877, 3.740497495074990297E-15, 475.6392848759629715 ) ) ;
#2939 = CARTESIAN_POINT ( 'NONE',  ( -68.63039925413394826, 1.572093150103981429E-15, 524.1455590405157636 ) ) ;
#2940 = CARTESIAN_POINT ( 'NONE',  ( -364.1439395362590972, 2.398458366376004494E-13, 237.2787335496881553 ) ) ;
#2941 = COLOUR_RGB ( '',0.7921568627450980005, 0.8196078431372548767, 0.9333333333333333481 ) ;
#2942 = AXIS2_PLACEMENT_3D ( 'NONE', #3778, #429, #3840 ) ;
#2943 = VERTEX_POINT ( 'NONE', #676 ) ;
#2944 = EDGE_CURVE ( 'NONE', #2425, #483, #2714, .T. ) ;
#2945 = CARTESIAN_POINT ( 'NONE',  ( -317.5233545270529021, 6.019019530952224355E-15, 141.2297481720574126 ) ) ;
#2946 = ADVANCED_FACE ( 'NONE', ( #3400 ), #5053, .F. ) ;
#2947 = COLOUR_RGB ( '',0.7921568627450980005, 0.8196078431372548767, 0.9333333333333333481 ) ;
#2948 = ORIENTED_EDGE ( 'NONE', *, *, #4694, .T. ) ;
#2949 = CARTESIAN_POINT ( 'NONE',  ( -77.37696704867103392, -26.07682022631158247, -10.00000000000000888 ) ) ;
#2950 = DIRECTION ( 'NONE',  ( 0.4205749795070158337, 0.9072577839912276954, 0.000000000000000000 ) ) ;
#2951 = LINE ( 'NONE', #857, #1699 ) ;
#2952 = CARTESIAN_POINT ( 'NONE',  ( 137.9714219172561513, -25.54565493204318116, -11.99999999999995559 ) ) ;
#2953 = CARTESIAN_POINT ( 'NONE',  ( 29.23877717791895492, 0.000000000000000000, 67.09613410133256650 ) ) ;
#2954 = ORIENTED_EDGE ( 'NONE', *, *, #1046, .F. ) ;
#2955 = ORIENTED_EDGE ( 'NONE', *, *, #4038, .T. ) ;
#2956 = EDGE_LOOP ( 'NONE', ( #3458, #4428, #4965, #2555, #5388, #3851, #755, #5084 ) ) ;
#2957 = CARTESIAN_POINT ( 'NONE',  ( -316.5277671734493197, 2.222614453595266735E-15, 141.3235875099962584 ) ) ;
#2958 = CYLINDRICAL_SURFACE ( 'NONE', #2829, 4.382543221487789964 ) ;
#2959 = CARTESIAN_POINT ( 'NONE',  ( -344.9797493358575480, 2.222614453595284090E-15, 107.5044404032142751 ) ) ;
#2960 = CARTESIAN_POINT ( 'NONE',  ( -338.5048350180761076, 2.276824562219559311E-15, 38.80891300457378890 ) ) ;
#2961 = AXIS2_PLACEMENT_3D ( 'NONE', #1035, #1889, #1418 ) ;
#2962 = CARTESIAN_POINT ( 'NONE',  ( 96.73877717791896202, -14.99999999999998579, 67.09613410133256650 ) ) ;
#2963 = CARTESIAN_POINT ( 'NONE',  ( -167.9289969670495282, -24.99999999999981881, 528.5729890193230176 ) ) ;
#2964 = CARTESIAN_POINT ( 'NONE',  ( -360.7307227603793649, 2.222614453595284090E-15, 354.4373729494858480 ) ) ;
#2965 = AXIS2_PLACEMENT_3D ( 'NONE', #4467, #3652, #1576 ) ;
#2966 = ORIENTED_EDGE ( 'NONE', *, *, #1435, .F. ) ;
#2967 = ORIENTED_EDGE ( 'NONE', *, *, #1605, .F. ) ;
#2968 = CARTESIAN_POINT ( 'NONE',  ( -84.02857808274413287, 84.45434506795682239, -5.551115123125782702E-14 ) ) ;
#2969 = DIRECTION ( 'NONE',  ( 1.000000000000000000, 0.000000000000000000, 0.000000000000000000 ) ) ;
#2970 = AXIS2_PLACEMENT_3D ( 'NONE', #4313, #3575, #541 ) ;
#2971 = VERTEX_POINT ( 'NONE', #3547 ) ;
#2972 = CYLINDRICAL_SURFACE ( 'NONE', #4085, 4.382543221487789964 ) ;
#2973 = VERTEX_POINT ( 'NONE', #701 ) ;
#2974 = DIRECTION ( 'NONE',  ( 5.551115123125772841E-17, -1.848892746611743135E-31, -1.000000000000000000 ) ) ;
#2975 = DIRECTION ( 'NONE',  ( 5.551115123125772841E-17, -1.848892746611743135E-31, -1.000000000000000000 ) ) ;
#2976 = DIRECTION ( 'NONE',  ( 1.000000000000000000, 1.261617073437686134E-16, 5.551115123125772841E-17 ) ) ;
#2977 = CARTESIAN_POINT ( 'NONE',  ( 133.9714219172562366, -21.54565493204319182, -2.000000000000001776 ) ) ;
#2978 = DIRECTION ( 'NONE',  ( 1.000000000000000000, -5.777789833161702304E-31, 0.000000000000000000 ) ) ;
#2979 = ORIENTED_EDGE ( 'NONE', *, *, #4135, .F. ) ;
#2980 = ORIENTED_EDGE ( 'NONE', *, *, #2910, .F. ) ;
#2981 = EDGE_CURVE ( 'NONE', #4519, #1066, #5111, .T. ) ;
#2982 = EDGE_CURVE ( 'NONE', #249, #2943, #3578, .T. ) ;
#2983 = ORIENTED_EDGE ( 'NONE', *, *, #4316, .T. ) ;
#2984 = CARTESIAN_POINT ( 'NONE',  ( 96.73877717791896202, 0.000000000000000000, 131.6034880481681171 ) ) ;
#2985 = ADVANCED_FACE ( 'NONE', ( #2358 ), #3250, .F. ) ;
#2986 = DIRECTION ( 'NONE',  ( 0.09383933793885537722, -2.626968444144180508E-31, -0.9955873536034883786 ) ) ;
#2987 = FACE_OUTER_BOUND ( 'NONE', #2257, .T. ) ;
#2988 = ADVANCED_FACE ( 'NONE', ( #3661 ), #2385, .F. ) ;
#2989 =( LENGTH_UNIT ( ) NAMED_UNIT ( * ) SI_UNIT ( .MILLI., .METRE. ) );
#2990 = ORIENTED_EDGE ( 'NONE', *, *, #5271, .F. ) ;
#2991 = CARTESIAN_POINT ( 'NONE',  ( -339.2542556961718674, -2.870467298361735770E-14, 239.6247169981594141 ) ) ;
#2992 = CARTESIAN_POINT ( 'NONE',  ( -213.0979982360503584, 1.517883041479706208E-15, 511.7519955242227070 ) ) ;
#2993 = DIRECTION ( 'NONE',  ( 5.551115123125772841E-17, -1.848892746611743354E-31, -1.000000000000000000 ) ) ;
#2994 = ORIENTED_EDGE ( 'NONE', *, *, #695, .F. ) ;
#2995 = ORIENTED_EDGE ( 'NONE', *, *, #2682, .T. ) ;
#2996 = DIRECTION ( 'NONE',  ( 4.476705744456277327E-17, 0.000000000000000000, 1.000000000000000000 ) ) ;
#2997 = LINE ( 'NONE', #3828, #4342 ) ;
#2998 = ADVANCED_FACE ( 'NONE', ( #5321 ), #4907, .T. ) ;
#2999 = EDGE_CURVE ( 'NONE', #2650, #486, #5023, .T. ) ;
#3000 = EDGE_LOOP ( 'NONE', ( #4914, #3617, #782, #2832 ) ) ;
#3001 = CARTESIAN_POINT ( 'NONE',  ( -378.3480224348070351, 2.222614453595300656E-15, 136.5011359113908611 ) ) ;
#3002 = EDGE_CURVE ( 'NONE', #964, #4350, #4369, .T. ) ;
#3003 = CARTESIAN_POINT ( 'NONE',  ( -80.02857808274418971, -21.54565493204321669, -2.000000000000001776 ) ) ;
#3004 = CARTESIAN_POINT ( 'NONE',  ( -86.97194166595129161, 3.740497495074990297E-15, 531.0655262460708173 ) ) ;
#3005 = FILL_AREA_STYLE_COLOUR ( '', #3561 ) ;
#3006 = CARTESIAN_POINT ( 'NONE',  ( 35.78913469918423829, 0.000000000000000000, 310.6402212931345161 ) ) ;
#3007 = PRODUCT ( 'MAT-023', 'MAT-023', '', ( #621 ) ) ;
#3008 = CARTESIAN_POINT ( 'NONE',  ( -60.76122282208098824, -14.99999999999998579, 167.0961341013325523 ) ) ;
#3009 = AXIS2_PLACEMENT_3D ( 'NONE', #608, #3072, #3460 ) ;
#3010 = ORIENTED_EDGE ( 'NONE', *, *, #4064, .T. ) ;
#3011 = ORIENTED_EDGE ( 'NONE', *, *, #4316, .F. ) ;
#3012 = AXIS2_PLACEMENT_3D ( 'NONE', #5080, #2045, #3725 ) ;
#3013 = VERTEX_POINT ( 'NONE', #1119 ) ;
#3014 = LINE ( 'NONE', #2705, #4777 ) ;
#3015 = DIRECTION ( 'NONE',  ( 0.9955873536034882676, 0.000000000000000000, 0.09383933793885600172 ) ) ;
#3016 = DIRECTION ( 'NONE',  ( -1.000000000000000000, 0.000000000000000000, 0.000000000000000000 ) ) ;
#3017 = EDGE_CURVE ( 'NONE', #4129, #3237, #3894, .T. ) ;
#3018 = AXIS2_PLACEMENT_3D ( 'NONE', #299, #3954, #1531 ) ;
#3019 = CIRCLE ( 'NONE', #4680, 14.00000000000002665 ) ;
#3020 = FILL_AREA_STYLE ('',( #2633 ) ) ;
#3021 = EDGE_LOOP ( 'NONE', ( #1516, #1044 ) ) ;
#3022 = ADVANCED_FACE ( 'NONE', ( #1659 ), #4969, .F. ) ;
#3023 = CARTESIAN_POINT ( 'NONE',  ( -198.3455225866217404, 1.517883041479706208E-15, 518.3576047634792303 ) ) ;
#3024 = AXIS2_PLACEMENT_3D ( 'NONE', #2446, #2860, #3707 ) ;
#3025 = CARTESIAN_POINT ( 'NONE',  ( 4.992201166475765284, -24.99999999999981881, 252.6216919286950429 ) ) ;
#3026 = CARTESIAN_POINT ( 'NONE',  ( -354.9469840587070735, 2.222614453595298289E-15, 100.5383829474108524 ) ) ;
#3027 = AXIS2_PLACEMENT_3D ( 'NONE', #1572, #1104, #5222 ) ;
#3028 = VECTOR ( 'NONE', #2085, 1000.000000000000000 ) ;
#3029 = ORIENTED_EDGE ( 'NONE', *, *, #3318, .T. ) ;
#3030 = ORIENTED_EDGE ( 'NONE', *, *, #3479, .T. ) ;
#3031 = CARTESIAN_POINT ( 'NONE',  ( -78.28422483266214726, 85.40608534173227895, -12.00000000000001066 ) ) ;
#3032 = PRESENTATION_LAYER_ASSIGNMENT (  '', '', ( #3477 ) ) ;
#3033 =( NAMED_UNIT ( * ) PLANE_ANGLE_UNIT ( ) SI_UNIT ( $, .RADIAN. ) );
#3034 = AXIS2_PLACEMENT_3D ( 'NONE', #3059, #4269, #1752 ) ;
#3035 = AXIS2_PLACEMENT_3D ( 'NONE', #5349, #4446, #674 ) ;
#3036 = VECTOR ( 'NONE', #2051, 1000.000000000000000 ) ;
#3037 = ORIENTED_EDGE ( 'NONE', *, *, #4537, .T. ) ;
#3038 = CARTESIAN_POINT ( 'NONE',  ( 34.60640066538633874, 2.222614453595284090E-15, 295.6817845355787995 ) ) ;
#3039 = LINE ( 'NONE', #940, #3201 ) ;
#3040 = CARTESIAN_POINT ( 'NONE',  ( -336.1069982926114221, -24.99999999999981881, 349.6877309229307684 ) ) ;
#3041 = CARTESIAN_POINT ( 'NONE',  ( -156.9923520473269321, 0.000000000000000000, 556.8176423728721147 ) ) ;
#3042 = DIRECTION ( 'NONE',  ( -0.9955873536034882676, 5.484003909441382024E-31, -0.09383933793885569641 ) ) ;
#3043 = AXIS2_PLACEMENT_3D ( 'NONE', #324, #2381, #1998 ) ;
#3044 = ORIENTED_EDGE ( 'NONE', *, *, #618, .T. ) ;
#3045 = ORIENTED_EDGE ( 'NONE', *, *, #961, .T. ) ;
#3046 = ORIENTED_EDGE ( 'NONE', *, *, #4729, .F. ) ;
#3047 = FACE_BOUND ( 'NONE', #1213, .T. ) ;
#3048 = CARTESIAN_POINT ( 'NONE',  ( -347.8887688119608015, 2.222614453595284090E-15, 138.3676483649225588 ) ) ;
#3049 = LINE ( 'NONE', #4721, #1348 ) ;
#3050 = DIRECTION ( 'NONE',  ( -0.09383933793885568253, 2.673190762809473730E-31, 0.9955873536034882676 ) ) ;
#3051 = EDGE_LOOP ( 'NONE', ( #5273, #2205 ) ) ;
#3052 = SHAPE_REPRESENTATION ( 'Conveyor Speed Sensor Mount', ( #2926 ), #2227 ) ;
#3053 = DIRECTION ( 'NONE',  ( -0.4205749795070158337, -0.9072577839912276954, 0.000000000000000000 ) ) ;
#3054 = CARTESIAN_POINT ( 'NONE',  ( 31.14585677005056041, -24.99999999999981881, 398.7793066466517757 ) ) ;
#3055 = CARTESIAN_POINT ( 'NONE',  ( -82.68018911681718919, 75.92317977368848858, -12.00000000000001066 ) ) ;
#3056 = ORIENTED_EDGE ( 'NONE', *, *, #3232, .T. ) ;
#3057 = ADVANCED_FACE ( 'NONE', ( #379 ), #2082, .F. ) ;
#3058 = LINE ( 'NONE', #4346, #770 ) ;
#3059 = CARTESIAN_POINT ( 'NONE',  ( -346.0119820531829191, 0.000000000000000000, 118.4559012928527721 ) ) ;
#3060 = EDGE_CURVE ( 'NONE', #1068, #339, #2841, .T. ) ;
#3061 = ORIENTED_EDGE ( 'NONE', *, *, #3329, .F. ) ;
#3062 = CARTESIAN_POINT ( 'NONE',  ( -320.6447527397726276, 2.276824562219559311E-15, 453.8399743637901906 ) ) ;
#3063 = CARTESIAN_POINT ( 'NONE',  ( -84.02857808274403340, 98.45434506795682239, -12.00000000000001066 ) ) ;
#3064 = CARTESIAN_POINT ( 'NONE',  ( -68.63039925413394826, 1.572093150103981429E-15, 524.1455590405157636 ) ) ;
#3065 = CARTESIAN_POINT ( 'NONE',  ( 132.2270686671745352, 85.40608534173219368, -11.99999999999995559 ) ) ;
#3066 = CARTESIAN_POINT ( 'NONE',  ( -349.8593949086763928, 2.222614453595284090E-15, 159.2749827905956010 ) ) ;
#3067 = PRODUCT_RELATED_PRODUCT_CATEGORY ( 'part', '', ( #1704 ) ) ;
#3068 = VERTEX_POINT ( 'NONE', #814 ) ;
#3069 = VERTEX_POINT ( 'NONE', #4535 ) ;
#3070 = ORIENTED_EDGE ( 'NONE', *, *, #2679, .T. ) ;
#3071 = DIRECTION ( 'NONE',  ( -1.000000000000000000, 3.759415251443877379E-31, -5.551115123125772841E-17 ) ) ;
#3072 = DIRECTION ( 'NONE',  ( 0.000000000000000000, 1.000000000000000000, 0.000000000000000000 ) ) ;
#3073 = DIRECTION ( 'NONE',  ( -0.9955873536034883786, 5.496925049605202091E-31, -0.09383933793885522456 ) ) ;
#3074 =( NAMED_UNIT ( * ) SI_UNIT ( $, .STERADIAN. ) SOLID_ANGLE_UNIT ( ) );
#3075 = VERTEX_POINT ( 'NONE', #846 ) ;
#3076 = LINE ( 'NONE', #2270, #5057 ) ;
#3077 = CARTESIAN_POINT ( 'NONE',  ( -285.5643670724624599, -25.00000000000003197, 494.2304181244473966 ) ) ;
#3078 = CARTESIAN_POINT ( 'NONE',  ( -351.6990976162155107, 2.276824562219559311E-15, 238.4517252739237847 ) ) ;
#3079 = SHAPE_REPRESENTATION ( 'Stainless Steel Outer Shield Cover', ( #2926 ), #574 ) ;
#3080 = ORIENTED_EDGE ( 'NONE', *, *, #1906, .F. ) ;
#3081 = CARTESIAN_POINT ( 'NONE',  ( -334.2906958041416488, 0.000000000000000000, 430.9840019716568804 ) ) ;
#3082 = CARTESIAN_POINT ( 'NONE',  ( 2.673134346766241176, -0.2680804068607387514, 307.6774225009002635 ) ) ;
#3083 = EDGE_CURVE ( 'NONE', #4995, #2687, #471, .T. ) ;
#3084 = EDGE_CURVE ( 'NONE', #2803, #895, #386, .T. ) ;
#3085 = ORIENTED_EDGE ( 'NONE', *, *, #1605, .T. ) ;
#3086 = CARTESIAN_POINT ( 'NONE',  ( 12.58979647763672283, 2.222614453595284090E-15, 97.46177917736021357 ) ) ;
#3087 = ORIENTED_EDGE ( 'NONE', *, *, #4702, .F. ) ;
#3088 = EDGE_CURVE ( 'NONE', #4329, #911, #5026, .T. ) ;
#3089 = ADVANCED_FACE ( 'NONE', ( #788 ), #2884, .F. ) ;
#3090 = CARTESIAN_POINT ( 'NONE',  ( 159.4907110033991273, 15.00000000000001421, 139.1303977902171596 ) ) ;
#3091 = DIRECTION ( 'NONE',  ( 0.9072577839912278064, -0.4205749795070158892, -5.551115123125773458E-17 ) ) ;
#3092 = DIRECTION ( 'NONE',  ( 5.551115123125772841E-17, -1.848892746611743135E-31, -1.000000000000000000 ) ) ;
#3093 = ORIENTED_EDGE ( 'NONE', *, *, #4921, .F. ) ;
#3094 = UNCERTAINTY_MEASURE_WITH_UNIT (LENGTH_MEASURE( 1.000000000000000082E-05 ), #852, 'distance_accuracy_value', 'NONE');
#3095 = VERTEX_POINT ( 'NONE', #1229 ) ;
#3096 = CARTESIAN_POINT ( 'NONE',  ( -366.9888585194556754, 2.222614453595296317E-15, 99.40337302301857392 ) ) ;
#3097 = CARTESIAN_POINT ( 'NONE',  ( -346.1058213911226176, 0.000000000000000000, 119.4514886464559424 ) ) ;
#3098 = CARTESIAN_POINT ( 'NONE',  ( 4.898587196589413815E-15, 0.000000000000000000, 40.00000000000000000 ) ) ;
#3099 = DIRECTION ( 'NONE',  ( 0.09383933793885568253, -2.673190762809473730E-31, -0.9955873536034882676 ) ) ;
#3100 = VERTEX_POINT ( 'NONE', #4989 ) ;
#3101 = AXIS2_PLACEMENT_3D ( 'NONE', #4492, #718, #319 ) ;
#3102 = CARTESIAN_POINT ( 'NONE',  ( 133.9714219172562650, 80.45434506795682239, -9.999999999999841904 ) ) ;
#3103 = CARTESIAN_POINT ( 'NONE',  ( 11.81831109762766729, -25.00000000000000355, 46.95220429669349471 ) ) ;
#3104 = CYLINDRICAL_SURFACE ( 'NONE', #2062, 4.382543221487789964 ) ;
#3105 = CIRCLE ( 'NONE', #3794, 27.50000000000126832 ) ;
#3106 = AXIS2_PLACEMENT_3D ( 'NONE', #4975, #2806, #1154 ) ;
#3107 = AXIS2_PLACEMENT_3D ( 'NONE', #4440, #263, #2349 ) ;
#3108 = AXIS2_PLACEMENT_3D ( 'NONE', #4692, #514, #929 ) ;
#3109 = CARTESIAN_POINT ( 'NONE',  ( -347.8887688119603467, 2.222614453595284090E-15, 138.3676483649222178 ) ) ;
#3110 = CARTESIAN_POINT ( 'NONE',  ( 24.85474708473287109, 3.252606517456513302E-16, 216.1905617304896623 ) ) ;
#3111 = CARTESIAN_POINT ( 'NONE',  ( -21.24106685716701293, 85.96135828609807561, 14.10007152686019261 ) ) ;
#3112 = AXIS2_PLACEMENT_3D ( 'NONE', #687, #1510, #3209 ) ;
#3113 = VECTOR ( 'NONE', #1555, 1000.000000000000000 ) ;
#3114 = MANIFOLD_SOLID_BREP ( 'Boss-Extrude1', #2261 ) ;
#3115 = EDGE_LOOP ( 'NONE', ( #1459, #4978, #4964, #5152 ) ) ;
#3116 = CARTESIAN_POINT ( 'NONE',  ( -72.60637664584220374, 25.00000000000018474, 552.9197695054134556 ) ) ;
#3117 = EDGE_CURVE ( 'NONE', #3520, #1799, #3685, .T. ) ;
#3118 = ORIENTED_EDGE ( 'NONE', *, *, #1565, .T. ) ;
#3119 = AXIS2_PLACEMENT_3D ( 'NONE', #4976, #391, #1216 ) ;
#3120 = CIRCLE ( 'NONE', #4954, 28.50000000000127898 ) ;
#3121 = LINE ( 'NONE', #170, #2920 ) ;
#3122 = AXIS2_PLACEMENT_3D ( 'NONE', #1932, #318, #1164 ) ;
#3123 = CARTESIAN_POINT ( 'NONE',  ( -353.4921497144319460, 2.222614453595284090E-15, 38.40071206960160310 ) ) ;
#3124 = AXIS2_PLACEMENT_3D ( 'NONE', #3928, #588, #3073 ) ;
#3125 = ORIENTED_EDGE ( 'NONE', *, *, #1401, .T. ) ;
#3126 = MANIFOLD_SOLID_BREP ( 'Boss-Extrude1', #3332 ) ;
#3127 = VERTEX_POINT ( 'NONE', #2656 ) ;
#3128 = CARTESIAN_POINT ( 'NONE',  ( -349.6717162327985307, 3.252606517456513302E-16, 157.2838080833889194 ) ) ;
#3129 = FACE_OUTER_BOUND ( 'NONE', #1105, .T. ) ;
#3130 = LINE ( 'NONE', #4744, #3548 ) ;
#3131 = SURFACE_SIDE_STYLE ('',( #3971 ) ) ;
#3132 = ORIENTED_EDGE ( 'NONE', *, *, #4567, .T. ) ;
#3133 = CARTESIAN_POINT ( 'NONE',  ( 132.2270686671743647, -26.49739520581860575, -9.999999999999953815 ) ) ;
#3134 = CARTESIAN_POINT ( 'NONE',  ( 35.78913469918393275, -24.99999999999981881, 310.6402212931347435 ) ) ;
#3135 = DIRECTION ( 'NONE',  ( -0.09383933793885568253, 2.673190762809473730E-31, 0.9955873536034882676 ) ) ;
#3136 = MANIFOLD_SOLID_BREP ( 'Boss-Extrude11', #5419 ) ;
#3137 = DIRECTION ( 'NONE',  ( -0.9955873536034882676, 5.502656983963330823E-31, -0.09383933793885547436 ) ) ;
#3138 = ADVANCED_FACE ( 'NONE', ( #1827 ), #3812, .T. ) ;
#3139 = DIRECTION ( 'NONE',  ( -0.9955873536034883786, 5.430490990731020552E-31, -0.09383933793885548824 ) ) ;
#3140 = CARTESIAN_POINT ( 'NONE',  ( -57.28677601057280100, 3.252606517456513302E-16, 546.4981013186296650 ) ) ;
#3141 = DIRECTION ( 'NONE',  ( 0.3958995075709740297, 0.000000000000000000, 0.9182938418093961053 ) ) ;
#3142 = ORIENTED_EDGE ( 'NONE', *, *, #3827, .T. ) ;
#3143 = CARTESIAN_POINT ( 'NONE',  ( -367.0460729392618759, 0.000000000000000000, 268.0688838304710089 ) ) ;
#3144 = ORIENTED_EDGE ( 'NONE', *, *, #3232, .F. ) ;
#3145 = DIRECTION ( 'NONE',  ( -2.523234146875361914E-16, -1.000000000000000000, -1.456973175402238023E-31 ) ) ;
#3146 = FILL_AREA_STYLE_COLOUR ( '', #2753 ) ;
#3147 = CLOSED_SHELL ( 'NONE', ( #3057, #3524, #3994, #3175, #3162, #1375 ) ) ;
#3148 = ORIENTED_EDGE ( 'NONE', *, *, #560, .T. ) ;
#3149 = EDGE_LOOP ( 'NONE', ( #1590, #2544, #361, #1315 ) ) ;
#3150 = DIRECTION ( 'NONE',  ( -2.523234146875361914E-16, -1.000000000000000000, -1.456973175402238023E-31 ) ) ;
#3151 = DIRECTION ( 'NONE',  ( 0.9998833722232041143, -6.779273404243022909E-31, -0.01527226085271993737 ) ) ;
#3152 = LINE ( 'NONE', #976, #15 ) ;
#3153 = ADVANCED_FACE ( 'NONE', ( #3437 ), #3841, .F. ) ;
#3154 = DIRECTION ( 'NONE',  ( 5.551115123125772841E-17, -1.848892746611743354E-31, -1.000000000000000000 ) ) ;
#3155 = ADVANCED_FACE ( 'NONE', ( #1309 ), #97, .T. ) ;
#3156 = CARTESIAN_POINT ( 'NONE',  ( -85.27857808274411866, -21.54565493204320248, -26.84924240491759662 ) ) ;
#3157 = VERTEX_POINT ( 'NONE', #73 ) ;
#3158 = EDGE_CURVE ( 'NONE', #3905, #5368, #453, .T. ) ;
#3159 = ADVANCED_FACE ( 'NONE', ( #5125 ), #46, .F. ) ;
#3160 = SURFACE_STYLE_USAGE ( .BOTH. , #3975 ) ;
#3161 = LINE ( 'NONE', #2196, #3325 ) ;
#3162 = ADVANCED_FACE ( 'NONE', ( #1333 ), #3464, .T. ) ;
#3163 = CARTESIAN_POINT ( 'NONE',  ( 31.14585677005082687, 2.222614453595284090E-15, 398.7793066466531968 ) ) ;
#3164 = DIRECTION ( 'NONE',  ( 0.09383933793885125552, -2.549931246368697204E-31, -0.9955873536034887117 ) ) ;
#3165 = DIRECTION ( 'NONE',  ( -1.000000000000000000, 3.759415251443877379E-31, -5.551115123125772841E-17 ) ) ;
#3166 = DIRECTION ( 'NONE',  ( -0.9955873536034882676, 5.502656983963330823E-31, -0.09383933793885547436 ) ) ;
#3167 = CARTESIAN_POINT ( 'NONE',  ( 11.81831109762766729, 25.00000000000000355, 46.95220429669349471 ) ) ;
#3168 = APPLICATION_PROTOCOL_DEFINITION ( 'draft international standard', 'automotive_design', 1998, #5133 ) ;
#3169 = CARTESIAN_POINT ( 'NONE',  ( -35.15684241565268309, -24.99999999999981881, 493.9702760599490716 ) ) ;
#3170 = ORIENTED_EDGE ( 'NONE', *, *, #2271, .T. ) ;
#3171 = CARTESIAN_POINT ( 'NONE',  ( 8.821273309659243722, 25.00000000000018474, 380.5076279642384520 ) ) ;
#3172 = ORIENTED_EDGE ( 'NONE', *, *, #3084, .T. ) ;
#3173 = LINE ( 'NONE', #1070, #3979 ) ;
#3174 = PLANE ( 'NONE',  #1615 ) ;
#3175 = ADVANCED_FACE ( 'NONE', ( #2610, #538 ), #4722, .F. ) ;
#3176 = ADVANCED_FACE ( 'NONE', ( #237 ), #264, .T. ) ;
#3177 = ORIENTED_EDGE ( 'NONE', *, *, #224, .F. ) ;
#3178 = ORIENTED_EDGE ( 'NONE', *, *, #3496, .T. ) ;
#3179 = CARTESIAN_POINT ( 'NONE',  ( -48.13570084519473369, 0.000000000000000000, 62.68703548022111249 ) ) ;
#3180 = CARTESIAN_POINT ( 'NONE',  ( -338.5986743560152377, 2.276824562219559311E-15, 39.80450035817695209 ) ) ;
#3181 = DIRECTION ( 'NONE',  ( 0.000000000000000000, -0.000000000000000000, 1.000000000000000000 ) ) ;
#3182 = DIRECTION ( 'NONE',  ( 0.9955873536034882676, -5.499791016784056700E-31, 0.09383933793885550212 ) ) ;
#3183 = CYLINDRICAL_SURFACE ( 'NONE', #2408, 14.00000000000004086 ) ;
#3184 = EDGE_LOOP ( 'NONE', ( #1238, #1010 ) ) ;
#3185 = EDGE_CURVE ( 'NONE', #229, #1126, #4075, .T. ) ;
#3186 = CIRCLE ( 'NONE', #3536, 14.00000000000001243 ) ;
#3187 = CARTESIAN_POINT ( 'NONE',  ( 132.2270686671745068, 85.40608534173219368, -9.999999999999953815 ) ) ;
#3188 = CARTESIAN_POINT ( 'NONE',  ( -48.13570084519473369, 15.00000000000001421, 62.68703548022111249 ) ) ;
#3189 = EDGE_CURVE ( 'NONE', #3533, #1042, #1910, .T. ) ;
#3190 = CYLINDRICAL_SURFACE ( 'NONE', #2565, 27.43532828739476415 ) ;
#3191 = FACE_OUTER_BOUND ( 'NONE', #4462, .T. ) ;
#3192 = MANIFOLD_SOLID_BREP ( 'Cut-Extrude2', #4554 ) ;
#3193 = VECTOR ( 'NONE', #143, 1000.000000000000000 ) ;
#3194 = FACE_OUTER_BOUND ( 'NONE', #290, .T. ) ;
#3195 = AXIS2_PLACEMENT_3D ( 'NONE', #5221, #1509, #4048 ) ;
#3196 = DIRECTION ( 'NONE',  ( -0.9955873536034882676, 5.452307672560241053E-31, -0.09383933793885547436 ) ) ;
#3197 = CARTESIAN_POINT ( 'NONE',  ( -14.89480152442222582, 25.00000000000018474, 508.6517828409982940 ) ) ;
#3198 = DIRECTION ( 'NONE',  ( 0.9182938418093961053, 0.000000000000000000, -0.3958995075709740297 ) ) ;
#3199 = CARTESIAN_POINT ( 'NONE',  ( -339.2542556961722084, 3.740497495074990297E-15, 239.6247169981598972 ) ) ;
#3200 = CARTESIAN_POINT ( 'NONE',  ( -1.533280346156490337, 2.222614453595284090E-15, 488.4857301958385278 ) ) ;
#3201 = VECTOR ( 'NONE', #2623, 1000.000000000000000 ) ;
#3202 = CIRCLE ( 'NONE', #1515, 5.250000000000004441 ) ;
#3203 = EDGE_LOOP ( 'NONE', ( #2917, #4911, #1556, #2638 ) ) ;
#3204 = CARTESIAN_POINT ( 'NONE',  ( -39.32426838450110296, 25.00000000000018474, 499.4571537926176461 ) ) ;
#3205 = VERTEX_POINT ( 'NONE', #1031 ) ;
#3206 = CARTESIAN_POINT ( 'NONE',  ( -318.6333298290857101, -1.512095747587092168E-29, 121.0364830861714154 ) ) ;
#3207 = AXIS2_PLACEMENT_3D ( 'NONE', #565, #2288, #4281 ) ;
#3208 = COLOUR_RGB ( '',0.7921568627450980005, 0.8196078431372548767, 0.9333333333333333481 ) ;
#3209 = DIRECTION ( 'NONE',  ( -0.9998833722232041143, 6.779273404243020281E-31, 0.01527226085271993043 ) ) ;
#3210 = ORIENTED_EDGE ( 'NONE', *, *, #756, .T. ) ;
#3211 = PRODUCT_DEFINITION ( 'UNKNOWN', '', #1542, #2314 ) ;
#3212 = ORIENTED_EDGE ( 'NONE', *, *, #4594, .F. ) ;
#3213 = LINE ( 'NONE', #1107, #1074 ) ;
#3214 = DIRECTION ( 'NONE',  ( -0.9955873536034882676, 5.498529991225532962E-31, -0.09383933793885550212 ) ) ;
#3215 = CARTESIAN_POINT ( 'NONE',  ( -346.1058213911226176, 0.000000000000000000, 119.4514886464559424 ) ) ;
#3216 = DIRECTION ( 'NONE',  ( -0.9955873536034883786, 5.498529991225544347E-31, -0.09383933793885444741 ) ) ;
#3217 = AXIS2_PLACEMENT_3D ( 'NONE', #4881, #2796, #4475 ) ;
#3218 = CARTESIAN_POINT ( 'NONE',  ( -82.68018911681716077, -17.01448963777485446, -9.999999999999953815 ) ) ;
#3219 = ORIENTED_EDGE ( 'NONE', *, *, #1689, .T. ) ;
#3220 = CARTESIAN_POINT ( 'NONE',  ( -344.1351952944061168, 5.421010862427522170E-17, 98.54415422078321285 ) ) ;
#3221 = CYLINDRICAL_SURFACE ( 'NONE', #628, 39.24395386344908587 ) ;
#3222 = FACE_OUTER_BOUND ( 'NONE', #2871, .T. ) ;
#3223 = CARTESIAN_POINT ( 'NONE',  ( -78.28422483266226095, -26.49739520581859153, -12.00000000000006573 ) ) ;
#3224 = CYLINDRICAL_SURFACE ( 'NONE', #4023, 4.382543221487789964 ) ;
#3225 = CARTESIAN_POINT ( 'NONE',  ( -35.15684241565268309, 25.00000000000018474, 493.9702760599490716 ) ) ;
#3226 = CONTEXT_DEPENDENT_SHAPE_REPRESENTATION ( #2783, #45 ) ;
#3227 = CARTESIAN_POINT ( 'NONE',  ( 36.35777514575885760, 2.222614453595284090E-15, 354.7349908125909792 ) ) ;
#3228 = DIRECTION ( 'NONE',  ( -0.09383933793885568253, 2.673190762809473730E-31, 0.9955873536034882676 ) ) ;
#3229 = VERTEX_POINT ( 'NONE', #3598 ) ;
#3230 = CARTESIAN_POINT ( 'NONE',  ( -8.629236981538166873, 25.00000000000000355, 142.6115645898824198 ) ) ;
#3231 = ORIENTED_EDGE ( 'NONE', *, *, #2419, .F. ) ;
#3232 = EDGE_CURVE ( 'NONE', #4034, #4350, #1416, .T. ) ;
#3233 = ADVANCED_FACE ( 'NONE', ( #2267 ), #3949, .T. ) ;
#3234 = DIRECTION ( 'NONE',  ( -0.9998833722232041143, 6.779273404243020281E-31, 0.01527226085271993043 ) ) ;
#3235 = FACE_OUTER_BOUND ( 'NONE', #3115, .T. ) ;
#3236 = VERTEX_POINT ( 'NONE', #2709 ) ;
#3237 = VERTEX_POINT ( 'NONE', #4470 ) ;
#3238 = DIRECTION ( 'NONE',  ( 5.551115123125772841E-17, -1.848892746611743135E-31, -1.000000000000000000 ) ) ;
#3239 = CARTESIAN_POINT ( 'NONE',  ( 29.23877717791895492, -14.99999999999998579, 67.09613410133256650 ) ) ;
#3240 = LINE ( 'NONE', #4875, #3789 ) ;
#3241 = CARTESIAN_POINT ( 'NONE',  ( -351.6423423295148041, 5.421010862427522170E-17, 178.1911425090623311 ) ) ;
#3242 = AXIS2_PLACEMENT_3D ( 'NONE', #4448, #331, #3196 ) ;
#3243 = DIRECTION ( 'NONE',  ( -5.679099018122554920E-31, -1.000000000000000000, 2.149753974990777610E-31 ) ) ;
#3244 = ORIENTED_EDGE ( 'NONE', *, *, #275, .F. ) ;
#3245 = CARTESIAN_POINT ( 'NONE',  ( 0.000000000000000000, 0.000000000000000000, -40.00000000000000000 ) ) ;
#3246 = FACE_OUTER_BOUND ( 'NONE', #842, .T. ) ;
#3247 = CARTESIAN_POINT ( 'NONE',  ( -38.26122282208103798, -14.99999999999998579, 131.6034880481681171 ) ) ;
#3248 = DIRECTION ( 'NONE',  ( 0.09383933793885536334, -2.626968444144180070E-31, -0.9955873536034882676 ) ) ;
#3249 = AXIS2_PLACEMENT_3D ( 'NONE', #2107, #48, #3780 ) ;
#3250 = CYLINDRICAL_SURFACE ( 'NONE', #4593, 56.63911695420810588 ) ;
#3251 = CARTESIAN_POINT ( 'NONE',  ( -323.7051989975983588, 2.222614453595284090E-15, 41.20828864675230108 ) ) ;
#3252 = CARTESIAN_POINT ( 'NONE',  ( 0.07030049711781446997, 25.00000000000000355, 219.5055207296751689 ) ) ;
#3253 = CARTESIAN_POINT ( 'NONE',  ( -19.78983854945498422, 2.222614453595284090E-15, 515.1268587725810448 ) ) ;
#3254 =( REPRESENTATION_RELATIONSHIP ('NONE','NONE', #2124, #3079 ) REPRESENTATION_RELATIONSHIP_WITH_TRANSFORMATION ( #1588 )SHAPE_REPRESENTATION_RELATIONSHIP( ) );
#3255 = ORIENTED_EDGE ( 'NONE', *, *, #3355, .T. ) ;
#3256 = CARTESIAN_POINT ( 'NONE',  ( -354.3266237013165778, 25.00000000000018474, 381.2801272015587983 ) ) ;
#3257 = ORIENTED_EDGE ( 'NONE', *, *, #2933, .T. ) ;
#3258 = CARTESIAN_POINT ( 'NONE',  ( -320.2813406910036633, 5.421010862425789758E-17, 181.1470816541363718 ) ) ;
#3259 = ADVANCED_FACE ( 'NONE', ( #1053 ), #205, .T. ) ;
#3260 = CARTESIAN_POINT ( 'NONE',  ( -374.4264635139651887, 2.571758278209474793E-15, 196.1322634844163417 ) ) ;
#3261 = EDGE_CURVE ( 'NONE', #577, #1068, #5254, .T. ) ;
#3262 = ORIENTED_EDGE ( 'NONE', *, *, #2682, .F. ) ;
#3263 = EDGE_CURVE ( 'NONE', #1423, #3802, #307, .T. ) ;
#3264 = ORIENTED_EDGE ( 'NONE', *, *, #2582, .T. ) ;
#3265 = DIRECTION ( 'NONE',  ( -1.000000000000000000, 0.000000000000000000, 0.000000000000000000 ) ) ;
#3266 = DIRECTION ( 'NONE',  ( -5.551115123125772841E-17, 1.848892746611743135E-31, 1.000000000000000000 ) ) ;
#3267 = LINE ( 'NONE', #4090, #5104 ) ;
#3268 = CARTESIAN_POINT ( 'NONE',  ( -319.5145292342597827, 5.712857831165349408E-15, 141.0420694961801189 ) ) ;
#3269 = CARTESIAN_POINT ( 'NONE',  ( 133.9714219172562366, 80.45434506795683660, -12.00000000000001066 ) ) ;
#3270 = ORIENTED_EDGE ( 'NONE', *, *, #1722, .T. ) ;
#3271 = FACE_OUTER_BOUND ( 'NONE', #169, .T. ) ;
#3272 = FACE_OUTER_BOUND ( 'NONE', #2254, .T. ) ;
#3273 = CARTESIAN_POINT ( 'NONE',  ( 29.23877717791895492, -14.99999999999998579, 67.09613410133256650 ) ) ;
#3274 = CARTESIAN_POINT ( 'NONE',  ( -98.02857808274411866, 84.45434506795672291, 5.551115123125782702E-14 ) ) ;
#3275 = FILL_AREA_STYLE_COLOUR ( '', #3722 ) ;
#3276 = CIRCLE ( 'NONE', #1061, 50.00000000000000000 ) ;
#3277 = FACE_BOUND ( 'NONE', #4489, .T. ) ;
#3278 = CARTESIAN_POINT ( 'NONE',  ( -12.39202333278749357, 1.572093150103981429E-15, 98.84296066633379496 ) ) ;
#3279 = CARTESIAN_POINT ( 'NONE',  ( -174.3534642324304116, 5.421010862427522170E-17, 552.7876087698471110 ) ) ;
#3280 = AXIS2_PLACEMENT_3D ( 'NONE', #3927, #2707, #564 ) ;
#3281 = VERTEX_POINT ( 'NONE', #3572 ) ;
#3282 = CARTESIAN_POINT ( 'NONE',  ( 0.07030049711781446997, 25.00000000000000355, 219.5055207296751689 ) ) ;
#3283 = ORIENTED_EDGE ( 'NONE', *, *, #4790, .T. ) ;
#3284 = AXIS2_PLACEMENT_3D ( 'NONE', #779, #3796, #1707 ) ;
#3285 = CARTESIAN_POINT ( 'NONE',  ( 96.73877717791896202, -14.99999999999998579, 67.09613410133256650 ) ) ;
#3286 = CARTESIAN_POINT ( 'NONE',  ( -84.02857808274397655, -39.54565493204319893, 152.0000000000000853 ) ) ;
#3287 = VECTOR ( 'NONE', #2119, 1000.000000000000000 ) ;
#3288 = EDGE_CURVE ( 'NONE', #3474, #2151, #29, .T. ) ;
#3289 = ORIENTED_EDGE ( 'NONE', *, *, #4132, .F. ) ;
#3290 = CIRCLE ( 'NONE', #5115, 67.50000000000001421 ) ;
#3291 = AXIS2_PLACEMENT_3D ( 'NONE', #2032, #5375, #2104 ) ;
#3292 = EDGE_LOOP ( 'NONE', ( #1923, #3695, #1524, #436 ) ) ;
#3293 = CARTESIAN_POINT ( 'NONE',  ( -351.6990976162155107, 2.276824562219559311E-15, 238.4517252739237847 ) ) ;
#3294 = DIRECTION ( 'NONE',  ( -0.9955873536034882676, 5.484003909441392533E-31, -0.09383933793885569641 ) ) ;
#3295 = CARTESIAN_POINT ( 'NONE',  ( 132.2270686671745068, 85.40608534173219368, -9.999999999999953815 ) ) ;
#3296 = CARTESIAN_POINT ( 'NONE',  ( -77.37696704867103392, -26.07682022631158247, -10.00000000000000888 ) ) ;
#3297 = AXIS2_PLACEMENT_3D ( 'NONE', #1547, #4111, #1463 ) ;
#3298 = CIRCLE ( 'NONE', #3730, 5.250000000000004441 ) ;
#3299 = LINE ( 'NONE', #4145, #5124 ) ;
#3300 = ORIENTED_EDGE ( 'NONE', *, *, #2008, .F. ) ;
#3301 = ADVANCED_FACE ( 'NONE', ( #2289 ), #3183, .T. ) ;
#3302 = ORIENTED_EDGE ( 'NONE', *, *, #4878, .T. ) ;
#3303 = CARTESIAN_POINT ( 'NONE',  ( -353.4252897503525332, 0.000000000000000000, 197.1073022275279243 ) ) ;
#3304 = CARTESIAN_POINT ( 'NONE',  ( -108.3530091724271358, 0.000000000000000000, 123.8676211295743599 ) ) ;
#3305 = DIRECTION ( 'NONE',  ( -1.000000000000000000, 3.759415251443877817E-31, -5.551115123125772841E-17 ) ) ;
#3306 = CIRCLE ( 'NONE', #4344, 31.50000000000125766 ) ;
#3307 = CIRCLE ( 'NONE', #4518, 39.24395386344908587 ) ;
#3308 = DIRECTION ( 'NONE',  ( 5.551115123125772841E-17, -1.848892746611743354E-31, -1.000000000000000000 ) ) ;
#3309 = AXIS2_PLACEMENT_3D ( 'NONE', #548, #599, #5161 ) ;
#3310 = CARTESIAN_POINT ( 'NONE',  ( -84.02857808274407603, -25.54565493204318116, 152.0000000000000853 ) ) ;
#3311 = CARTESIAN_POINT ( 'NONE',  ( 6.585909452840001954, 25.00000000000018474, 393.9228865916072664 ) ) ;
#3312 = CARTESIAN_POINT ( 'NONE',  ( -19.78983854945535725, -24.99999999999981881, 515.1268587725797943 ) ) ;
#3313 = ORIENTED_EDGE ( 'NONE', *, *, #3501, .T. ) ;
#3314 = VERTEX_POINT ( 'NONE', #1081 ) ;
#3315 = DIRECTION ( 'NONE',  ( 0.09383933793885537722, -2.626968444144180508E-31, -0.9955873536034883786 ) ) ;
#3316 = DIRECTION ( 'NONE',  ( 1.000000000000000000, 0.000000000000000000, 0.000000000000000000 ) ) ;
#3317 = ORIENTED_EDGE ( 'NONE', *, *, #5333, .T. ) ;
#3318 = EDGE_CURVE ( 'NONE', #3404, #3520, #2586, .T. ) ;
#3319 = PLANE ( 'NONE',  #1561 ) ;
#3320 = CYLINDRICAL_SURFACE ( 'NONE', #3012, 6.000000000000032863 ) ;
#3321 = FACE_OUTER_BOUND ( 'NONE', #497, .T. ) ;
#3322 = ORIENTED_EDGE ( 'NONE', *, *, #3827, .F. ) ;
#3323 = ORIENTED_EDGE ( 'NONE', *, *, #2852, .F. ) ;
#3324 = CARTESIAN_POINT ( 'NONE',  ( -80.02857808274401918, 80.45434506795689344, -12.00000000000001066 ) ) ;
#3325 = VECTOR ( 'NONE', #1808, 1000.000000000000000 ) ;
#3326 = FACE_OUTER_BOUND ( 'NONE', #1548, .T. ) ;
#3327 = CARTESIAN_POINT ( 'NONE',  ( 133.9714219172562366, -21.54565493204319182, -12.00000000000006573 ) ) ;
#3328 = EDGE_CURVE ( 'NONE', #3802, #1788, #4119, .T. ) ;
#3329 = EDGE_CURVE ( 'NONE', #3835, #251, #1697, .T. ) ;
#3330 = DIRECTION ( 'NONE',  ( 0.000000000000000000, 0.000000000000000000, 1.000000000000000000 ) ) ;
#3331 = EDGE_CURVE ( 'NONE', #2285, #832, #881, .T. ) ;
#3332 = CLOSED_SHELL ( 'NONE', ( #4196, #692, #2110, #4459, #1942, #4552 ) ) ;
#3333 = EDGE_CURVE ( 'NONE', #251, #3835, #4773, .T. ) ;
#3334 = CARTESIAN_POINT ( 'NONE',  ( -80.59222536594906217, 3.740497495074990297E-15, 529.1597157429033587 ) ) ;
#3335 = CARTESIAN_POINT ( 'NONE',  ( -299.8611223228771792, 24.99999999999997158, 439.6443911606498887 ) ) ;
#3336 = CARTESIAN_POINT ( 'NONE',  ( 5.624351423727524946, 2.222614453595284090E-15, 474.0483466084679662 ) ) ;
#3337 = CIRCLE ( 'NONE', #953, 6.000000000000032863 ) ;
#3338 = TOROIDAL_SURFACE ( 'NONE', #5335, 28.50000000000115818, 1.000000000000000000 ) ;
#3339 = VERTEX_POINT ( 'NONE', #3791 ) ;
#3340 = PRESENTATION_STYLE_ASSIGNMENT (( #2915 ) ) ;
#3341 = ORIENTED_EDGE ( 'NONE', *, *, #5175, .T. ) ;
#3342 = ORIENTED_EDGE ( 'NONE', *, *, #3060, .F. ) ;
#3343 = DIRECTION ( 'NONE',  ( 1.000000000000000000, 0.000000000000000000, 8.260587980841909197E-17 ) ) ;
#3344 = DIRECTION ( 'NONE',  ( 0.09383933793885568253, -2.673190762809473730E-31, -0.9955873536034882676 ) ) ;
#3345 = DIRECTION ( 'NONE',  ( 0.9998833722232040033, -6.797399803719615819E-31, -0.01527226085271964420 ) ) ;
#3346 = ADVANCED_FACE ( 'NONE', ( #3830 ), #2972, .T. ) ;
#3347 = DIRECTION ( 'NONE',  ( -1.000000000000000000, 0.000000000000000000, 0.000000000000000000 ) ) ;
#3348 = ORIENTED_EDGE ( 'NONE', *, *, #130, .T. ) ;
#3349 = ORIENTED_EDGE ( 'NONE', *, *, #1132, .T. ) ;
#3350 = FACE_OUTER_BOUND ( 'NONE', #373, .T. ) ;
#3351 = CARTESIAN_POINT ( 'NONE',  ( -81.77293133282591953, -16.59391465826784540, -11.99999999999995559 ) ) ;
#3352 = DIRECTION ( 'NONE',  ( 0.09383933793885568253, -2.673190762809473730E-31, -0.9955873536034882676 ) ) ;
#3353 = ADVANCED_FACE ( 'NONE', ( #4526 ), #59, .F. ) ;
#3354 = PRESENTATION_STYLE_ASSIGNMENT (( #2002 ) ) ;
#3355 = EDGE_CURVE ( 'NONE', #2877, #5050, #209, .T. ) ;
#3356 = CARTESIAN_POINT ( 'NONE',  ( -35.15684241565247703, 1.843143693225357538E-15, 493.9702760599520275 ) ) ;
#3357 = CARTESIAN_POINT ( 'NONE',  ( -0.4023372602957597799, 1.572093150103981429E-15, 421.4664991284013809 ) ) ;
#3358 = FACE_OUTER_BOUND ( 'NONE', #1025, .T. ) ;
#3359 = EDGE_LOOP ( 'NONE', ( #4311, #80, #2717, #190 ) ) ;
#3360 = AXIS2_PLACEMENT_3D ( 'NONE', #2683, #2265, #2654 ) ;
#3361 = DIRECTION ( 'NONE',  ( 0.4205749795070158337, 0.9072577839912276954, 0.000000000000000000 ) ) ;
#3362 = CARTESIAN_POINT ( 'NONE',  ( -318.7271691670245559, -1.485826063145656437E-29, 122.0320704397746709 ) ) ;
#3363 = VECTOR ( 'NONE', #2259, 999.9999999999998863 ) ;
#3364 = ORIENTED_EDGE ( 'NONE', *, *, #869, .F. ) ;
#3365 = CARTESIAN_POINT ( 'NONE',  ( 137.9714219172562935, -25.54565493204318116, 152.0000000000004263 ) ) ;
#3366 = AXIS2_PLACEMENT_3D ( 'NONE', #3613, #5270, #3511 ) ;
#3367 = CARTESIAN_POINT ( 'NONE',  ( -98.02857808274411866, 84.45434506795672291, 152.0000000000001990 ) ) ;
#3368 = AXIS2_PLACEMENT_3D ( 'NONE', #4521, #3675, #3265 ) ;
#3369 = DIRECTION ( 'NONE',  ( -5.551115123125772841E-17, 1.848892746611743135E-31, 1.000000000000000000 ) ) ;
#3370 = DIRECTION ( 'NONE',  ( -1.000000000000000000, 3.759415251443877817E-31, -5.551115123125772841E-17 ) ) ;
#3371 = PRODUCT_RELATED_PRODUCT_CATEGORY ( 'part', '', ( #2460 ) ) ;
#3372 = AXIS2_PLACEMENT_3D ( 'NONE', #3241, #640, #3182 ) ;
#3373 = ORIENTED_EDGE ( 'NONE', *, *, #2015, .T. ) ;
#3374 = EDGE_LOOP ( 'NONE', ( #1647, #539, #2076, #2431 ) ) ;
#3375 = CIRCLE ( 'NONE', #297, 6.000000000000032863 ) ;
#3376 = ORIENTED_EDGE ( 'NONE', *, *, #3158, .T. ) ;
#3377 = LINE ( 'NONE', #2493, #3036 ) ;
#3378 = DIRECTION ( 'NONE',  ( 5.551115123125772841E-17, -1.848892746611743135E-31, -1.000000000000000000 ) ) ;
#3379 = DIRECTION ( 'NONE',  ( -0.9955873536034882676, 5.452307672560245432E-31, -0.09383933793885568253 ) ) ;
#3380 = AXIS2_PLACEMENT_3D ( 'NONE', #3487, #5114, #5168 ) ;
#3381 = VECTOR ( 'NONE', #4152, 1000.000000000000000 ) ;
#3382 = VECTOR ( 'NONE', #2767, 1000.000000000000000 ) ;
#3383 = FILL_AREA_STYLE ('',( #3275 ) ) ;
#3384 = VECTOR ( 'NONE', #3491, 1000.000000000000000 ) ;
#3385 = CARTESIAN_POINT ( 'NONE',  ( 11.35554381053716000, 3.794707603699265519E-15, 353.5846600851142512 ) ) ;
#3386 = CARTESIAN_POINT ( 'NONE',  ( -48.20943979674346735, -24.99999999999981881, 509.2978244404901602 ) ) ;
#3387 = DIRECTION ( 'NONE',  ( -0.9983803615885645799, 0.000000000000000000, -0.05689159511111529371 ) ) ;
#3388 = AXIS2_PLACEMENT_3D ( 'NONE', #982, #182, #1857 ) ;
#3389 = ORIENTED_EDGE ( 'NONE', *, *, #4128, .F. ) ;
#3390 = VERTEX_POINT ( 'NONE', #1196 ) ;
#3391 = PLANE ( 'NONE',  #3034 ) ;
#3392 = AXIS2_PLACEMENT_3D ( 'NONE', #5227, #5250, #5277 ) ;
#3393 = DIRECTION ( 'NONE',  ( 0.09383933793885537722, -2.626968444144180508E-31, -0.9955873536034883786 ) ) ;
#3394 = EDGE_CURVE ( 'NONE', #5106, #1160, #1996, .T. ) ;
#3395 = EDGE_LOOP ( 'NONE', ( #2221, #4877 ) ) ;
#3396 = CARTESIAN_POINT ( 'NONE',  ( 151.9714219172562650, -25.54565493204307813, -11.99999999999995559 ) ) ;
#3397 = EDGE_CURVE ( 'NONE', #4488, #3530, #5051, .T. ) ;
#3398 = EDGE_CURVE ( 'NONE', #8, #2973, #735, .T. ) ;
#3399 = FACE_BOUND ( 'NONE', #1047, .T. ) ;
#3400 = FACE_OUTER_BOUND ( 'NONE', #4643, .T. ) ;
#3401 = DIRECTION ( 'NONE',  ( -0.9955873536034883786, 5.498529991225525955E-31, -0.09383933793885444741 ) ) ;
#3402 = FACE_BOUND ( 'NONE', #2202, .T. ) ;
#3403 = CARTESIAN_POINT ( 'NONE',  ( -84.02857808274407603, 84.45434506795682239, -11.99999999999995559 ) ) ;
#3404 = VERTEX_POINT ( 'NONE', #3701 ) ;
#3405 = ORIENTED_EDGE ( 'NONE', *, *, #1301, .F. ) ;
#3406 = CIRCLE ( 'NONE', #3106, 14.00000000000002665 ) ;
#3407 = EDGE_LOOP ( 'NONE', ( #3950, #2603, #3443, #413, #2112, #3070, #2879, #4798 ) ) ;
#3408 = CARTESIAN_POINT ( 'NONE',  ( 29.23877717791899755, 15.00000000000001421, 67.09613410133263756 ) ) ;
#3409 = DIRECTION ( 'NONE',  ( -0.09383933793885568253, 2.673190762809473730E-31, 0.9955873536034882676 ) ) ;
#3410 = CARTESIAN_POINT ( 'NONE',  ( -84.02857808274413287, 84.45434506795682239, 152.0000000000003126 ) ) ;
#3411 = DIRECTION ( 'NONE',  ( -0.09383933793885537722, 2.611561004589082621E-31, 0.9955873536034883786 ) ) ;
#3412 = ORIENTED_EDGE ( 'NONE', *, *, #1601, .F. ) ;
#3413 = CARTESIAN_POINT ( 'NONE',  ( -336.3653681801726520, -1.035187345108139271E-30, 239.8970098219878651 ) ) ;
#3414 = CARTESIAN_POINT ( 'NONE',  ( -12.39202333278750601, -25.00000000000000355, 98.84296066633362443 ) ) ;
#3415 = CARTESIAN_POINT ( 'NONE',  ( -345.9181427152443007, 2.222614453595284090E-15, 117.4603139392499429 ) ) ;
#3416 = EDGE_CURVE ( 'NONE', #3157, #5368, #3299, .T. ) ;
#3417 = EDGE_LOOP ( 'NONE', ( #2268, #2605, #4197, #4174 ) ) ;
#3418 = ORIENTED_EDGE ( 'NONE', *, *, #3989, .F. ) ;
#3419 = DIRECTION ( 'NONE',  ( 0.000000000000000000, 1.000000000000000000, 0.000000000000000000 ) ) ;
#3420 =( NAMED_UNIT ( * ) SI_UNIT ( $, .STERADIAN. ) SOLID_ANGLE_UNIT ( ) );
#3421 = DIRECTION ( 'NONE',  ( -0.9955873536034882676, 5.452307672560245432E-31, -0.09383933793885568253 ) ) ;
#3422 = EDGE_LOOP ( 'NONE', ( #4740, #1929, #3255, #1413 ) ) ;
#3423 = DIRECTION ( 'NONE',  ( -5.551115123125772841E-17, 1.848892746611743135E-31, 1.000000000000000000 ) ) ;
#3424 = EDGE_CURVE ( 'NONE', #5024, #2670, #3298, .T. ) ;
#3425 = CARTESIAN_POINT ( 'NONE',  ( -353.5191290882918338, 0.000000000000000000, 198.1028895811323025 ) ) ;
#3426 = CARTESIAN_POINT ( 'NONE',  ( 11.65205807320727871, -24.99999999999981881, 340.0738060255407049 ) ) ;
#3427 =( NAMED_UNIT ( * ) PLANE_ANGLE_UNIT ( ) SI_UNIT ( $, .RADIAN. ) );
#3428 = DIRECTION ( 'NONE',  ( 0.09383933793885537722, -2.626968444144180508E-31, -0.9955873536034883786 ) ) ;
#3429 = DIRECTION ( 'NONE',  ( -1.000000000000000000, -1.219242865862094703E-16, 0.000000000000000000 ) ) ;
#3430 = EDGE_CURVE ( 'NONE', #4488, #4657, #5344, .T. ) ;
#3431 = ORIENTED_EDGE ( 'NONE', *, *, #2777, .T. ) ;
#3432 = EDGE_LOOP ( 'NONE', ( #4323, #3080, #2870, #4825 ) ) ;
#3433 = ORIENTED_EDGE ( 'NONE', *, *, #1853, .F. ) ;
#3434 = FACE_OUTER_BOUND ( 'NONE', #3432, .T. ) ;
#3435 = LINE ( 'NONE', #3760, #2216 ) ;
#3436 = CARTESIAN_POINT ( 'NONE',  ( -346.1058213911226176, 0.000000000000000000, 119.4514886464559424 ) ) ;
#3437 = FACE_OUTER_BOUND ( 'NONE', #4569, .T. ) ;
#3438 = ORIENTED_EDGE ( 'NONE', *, *, #4229, .T. ) ;
#3439 = PLANE ( 'NONE',  #1829 ) ;
#3440 = CARTESIAN_POINT ( 'NONE',  ( 6.585909452865815084, -24.99999999999981881, 393.9228865916069253 ) ) ;
#3441 = DIRECTION ( 'NONE',  ( -0.09383933793885536334, 2.626968444144180070E-31, 0.9955873536034882676 ) ) ;
#3442 = CIRCLE ( 'NONE', #1055, 77.49999999999998579 ) ;
#3443 = ORIENTED_EDGE ( 'NONE', *, *, #4294, .T. ) ;
#3444 = ORIENTED_EDGE ( 'NONE', *, *, #2342, .T. ) ;
#3445 = CARTESIAN_POINT ( 'NONE',  ( -378.2336344863770705, 2.222614453595299473E-15, 156.6005616593380694 ) ) ;
#3446 = ORIENTED_EDGE ( 'NONE', *, *, #4533, .F. ) ;
#3447 = CARTESIAN_POINT ( 'NONE',  ( 36.66581985038887126, 25.00000000000018474, 340.1662229844756098 ) ) ;
#3448 = ORIENTED_EDGE ( 'NONE', *, *, #4860, .T. ) ;
#3449 = DIRECTION ( 'NONE',  ( -5.551115123125772841E-17, 1.848892746611743135E-31, 1.000000000000000000 ) ) ;
#3450 = CARTESIAN_POINT ( 'NONE',  ( -249.5207023207449879, -25.00000000000003197, 491.2832465756976035 ) ) ;
#3451 = CARTESIAN_POINT ( 'NONE',  ( 128.7214219172562082, 80.45434506795679397, -26.84924240491753977 ) ) ;
#3452 = LINE ( 'NONE', #5144, #1176 ) ;
#3453 = CIRCLE ( 'NONE', #5010, 5.250000000000018652 ) ;
#3454 = ADVANCED_BREP_SHAPE_REPRESENTATION ( '', ( #3126, #2926 ), #2227 ) ;
#3455 = ORIENTED_EDGE ( 'NONE', *, *, #3885, .F. ) ;
#3456 = ORIENTED_EDGE ( 'NONE', *, *, #2777, .F. ) ;
#3457 = AXIS2_PLACEMENT_3D ( 'NONE', #421, #369, #2463 ) ;
#3458 = ORIENTED_EDGE ( 'NONE', *, *, #618, .F. ) ;
#3459 = CYLINDRICAL_SURFACE ( 'NONE', #741, 4.382543221487789964 ) ;
#3460 = DIRECTION ( 'NONE',  ( 6.938893903907233308E-17, 0.000000000000000000, 1.000000000000000000 ) ) ;
#3461 = DIRECTION ( 'NONE',  ( 0.09383933793885537722, -2.626968444144180508E-31, -0.9955873536034883786 ) ) ;
#3462 = VECTOR ( 'NONE', #3449, 1000.000000000000000 ) ;
#3463 = VECTOR ( 'NONE', #2950, 1000.000000000000114 ) ;
#3464 = CYLINDRICAL_SURFACE ( 'NONE', #3108, 21.00000000000012790 ) ;
#3465 = ORIENTED_EDGE ( 'NONE', *, *, #4823, .T. ) ;
#3466 = ADVANCED_FACE ( 'NONE', ( #1579 ), #2152, .F. ) ;
#3467 = CIRCLE ( 'NONE', #1433, 1.000000000000000888 ) ;
#3468 = CARTESIAN_POINT ( 'NONE',  ( -353.3314504124138011, 0.000000000000000000, 196.1117148739250808 ) ) ;
#3469 = AXIS2_PLACEMENT_3D ( 'NONE', #1280, #3411, #4258 ) ;
#3470 = CARTESIAN_POINT ( 'NONE',  ( -249.5207023207449879, -25.00000000000003197, 491.2832465756976035 ) ) ;
#3471 = DIRECTION ( 'NONE',  ( -1.219242865862094703E-16, 1.000000000000000000, -1.149200448409289593E-17 ) ) ;
#3472 = AXIS2_PLACEMENT_3D ( 'NONE', #5081, #2260, #2626 ) ;
#3473 = VECTOR ( 'NONE', #3441, 1000.000000000000114 ) ;
#3474 = VERTEX_POINT ( 'NONE', #2594 ) ;
#3475 = ORIENTED_EDGE ( 'NONE', *, *, #1565, .F. ) ;
#3476 = CARTESIAN_POINT ( 'NONE',  ( 106.6132552010327288, 0.000000000000000000, 71.50523272244407735 ) ) ;
#3477=STYLED_ITEM('',(#5458),#1341);
#3478 = AXIS2_PLACEMENT_3D ( 'NONE', #2959, #409, #3379 ) ;
#3479 = EDGE_CURVE ( 'NONE', #3520, #3404, #1877, .T. ) ;
#3480 = ORIENTED_EDGE ( 'NONE', *, *, #3989, .T. ) ;
#3481 = CARTESIAN_POINT ( 'NONE',  ( -49.96441683051505578, 2.222614453595284090E-15, 542.4422122871075089 ) ) ;
#3482 = ORIENTED_EDGE ( 'NONE', *, *, #3333, .T. ) ;
#3483 = LINE ( 'NONE', #62, #723 ) ;
#3484 = LINE ( 'NONE', #2142, #4863 ) ;
#3485 = CARTESIAN_POINT ( 'NONE',  ( -167.9289969670495282, -24.99999999999981881, 528.5729890193230176 ) ) ;
#3486 = LINE ( 'NONE', #5143, #1677 ) ;
#3487 = CARTESIAN_POINT ( 'NONE',  ( -84.02857808274418971, -25.54565493204318116, -5.551115123125782702E-14 ) ) ;
#3488 = ORIENTED_EDGE ( 'NONE', *, *, #1935, .T. ) ;
#3489 = ORIENTED_EDGE ( 'NONE', *, *, #4050, .T. ) ;
#3490 = VERTEX_POINT ( 'NONE', #1701 ) ;
#3491 = DIRECTION ( 'NONE',  ( -0.000000000000000000, -1.000000000000000000, -0.000000000000000000 ) ) ;
#3492 = FACE_OUTER_BOUND ( 'NONE', #1384, .T. ) ;
#3493 = CARTESIAN_POINT ( 'NONE',  ( -374.4264635139651887, 2.571758278209474793E-15, 196.1322634844163417 ) ) ;
#3494 = ORIENTED_EDGE ( 'NONE', *, *, #1513, .T. ) ;
#3495 = DIRECTION ( 'NONE',  ( 0.000000000000000000, 0.000000000000000000, -1.000000000000000000 ) ) ;
#3496 = EDGE_CURVE ( 'NONE', #2476, #1072, #4271, .T. ) ;
#3497 = CARTESIAN_POINT ( 'NONE',  ( -264.1404626571541598, -25.00000000000003197, 511.7445549721641100 ) ) ;
#3498 = CYLINDRICAL_SURFACE ( 'NONE', #4603, 6.000000000000032863 ) ;
#3499 = EDGE_CURVE ( 'NONE', #5037, #2290, #4343, .T. ) ;
#3500 = ADVANCED_FACE ( 'NONE', ( #2409 ), #1833, .T. ) ;
#3501 = EDGE_CURVE ( 'NONE', #3639, #339, #3782, .T. ) ;
#3502 = ORIENTED_EDGE ( 'NONE', *, *, #1401, .F. ) ;
#3503 = CARTESIAN_POINT ( 'NONE',  ( -0.8482259245422840710, 2.276824562219559311E-15, 36.14439046289818691 ) ) ;
#3504 = PRODUCT_CONTEXT ( 'NONE', #3, 'mechanical' ) ;
#3505 = VECTOR ( 'NONE', #5416, 1000.000000000000000 ) ;
#3506 = AXIS2_PLACEMENT_3D ( 'NONE', #1862, #1478, #3139 ) ;
#3507 = EDGE_CURVE ( 'NONE', #3530, #3127, #3553, .T. ) ;
#3508 = ORIENTED_EDGE ( 'NONE', *, *, #3263, .F. ) ;
#3509 = CARTESIAN_POINT ( 'NONE',  ( 36.35777514575885760, 2.222614453595284090E-15, 354.7349908125909792 ) ) ;
#3510 = ORIENTED_EDGE ( 'NONE', *, *, #898, .F. ) ;
#3511 = DIRECTION ( 'NONE',  ( -0.9998833722232041143, 6.779273404243020281E-31, 0.01527226085271993043 ) ) ;
#3512 = CARTESIAN_POINT ( 'NONE',  ( -223.9642223310785312, 5.421010862427522170E-17, 534.3227077389987016 ) ) ;
#3513 = DIRECTION ( 'NONE',  ( 1.000000000000000000, 0.000000000000000000, 0.000000000000000000 ) ) ;
#3514 = TOROIDAL_SURFACE ( 'NONE', #1646, 28.50000000000115818, 1.000000000000000000 ) ;
#3515 = VERTEX_POINT ( 'NONE', #933 ) ;
#3516 = ORIENTED_EDGE ( 'NONE', *, *, #3397, .T. ) ;
#3517 = CARTESIAN_POINT ( 'NONE',  ( 29.23877717791895492, 0.000000000000000000, 117.0961341013325665 ) ) ;
#3518 = DIRECTION ( 'NONE',  ( -1.000000000000000000, 0.000000000000000000, 0.000000000000000000 ) ) ;
#3519 = DIRECTION ( 'NONE',  ( -0.09383933793885537722, 2.611561004589082621E-31, 0.9955873536034883786 ) ) ;
#3520 = VERTEX_POINT ( 'NONE', #4588 ) ;
#3521 = DIRECTION ( 'NONE',  ( 0.9998833722232041143, -6.779273404243020281E-31, -0.01527226085271993043 ) ) ;
#3522 = CARTESIAN_POINT ( 'NONE',  ( -339.2542556961734590, -24.99999999999981881, 239.6247169981589309 ) ) ;
#3523 = CARTESIAN_POINT ( 'NONE',  ( 136.6230329513293498, 75.92317977368846016, -11.99999999999995559 ) ) ;
#3524 = ADVANCED_FACE ( 'NONE', ( #4207 ), #2504, .T. ) ;
#3525 = PLANE ( 'NONE',  #2792 ) ;
#3526 = CARTESIAN_POINT ( 'NONE',  ( 23.50217280487988347, 25.00000000000018474, 428.9062724124379997 ) ) ;
#3527 = APPLICATION_PROTOCOL_DEFINITION ( 'draft international standard', 'automotive_design', 1998, #3 ) ;
#3528 = EDGE_LOOP ( 'NONE', ( #1484, #3475 ) ) ;
#3529 = CARTESIAN_POINT ( 'NONE',  ( -19.78983854945535725, 25.00000000000018474, 515.1268587725797943 ) ) ;
#3530 = VERTEX_POINT ( 'NONE', #434 ) ;
#3531 = DIRECTION ( 'NONE',  ( 0.000000000000000000, 0.000000000000000000, 1.000000000000000000 ) ) ;
#3532 = DIRECTION ( 'NONE',  ( -0.9955873536034882676, 5.406119142139367196E-31, -0.09383933793885596009 ) ) ;
#3533 = VERTEX_POINT ( 'NONE', #2614 ) ;
#3534 = UNCERTAINTY_MEASURE_WITH_UNIT (LENGTH_MEASURE( 1.000000000000000082E-05 ), #2989, 'distance_accuracy_value', 'NONE');
#3535 = EDGE_LOOP ( 'NONE', ( #4455, #3210, #2663, #3446 ) ) ;
#3536 = AXIS2_PLACEMENT_3D ( 'NONE', #4581, #1278, #3807 ) ;
#3537 = PLANE ( 'NONE',  #1530 ) ;
#3538 = CYLINDRICAL_SURFACE ( 'NONE', #807, 4.382543221487789964 ) ;
#3539 = DIRECTION ( 'NONE',  ( 0.000000000000000000, -1.000000000000000000, 0.000000000000000000 ) ) ;
#3540 = DIRECTION ( 'NONE',  ( 0.000000000000000000, 0.000000000000000000, -1.000000000000000000 ) ) ;
#3541 = VERTEX_POINT ( 'NONE', #2940 ) ;
#3542 = DIRECTION ( 'NONE',  ( -1.000000000000000000, 0.000000000000000000, 0.000000000000000000 ) ) ;
#3543 = CARTESIAN_POINT ( 'NONE',  ( -122.4270646331732451, -24.99999999999981881, 560.5113017241552598 ) ) ;
#3544 = FACE_OUTER_BOUND ( 'NONE', #3203, .T. ) ;
#3545 = CIRCLE ( 'NONE', #3886, 56.63911695420812009 ) ;
#3546 = AXIS2_PLACEMENT_3D ( 'NONE', #5363, #1599, #397 ) ;
#3547 = CARTESIAN_POINT ( 'NONE',  ( 135.7157751673381085, -16.59391465826787027, -9.999999999999953815 ) ) ;
#3548 = VECTOR ( 'NONE', #3539, 1000.000000000000000 ) ;
#3549=STYLED_ITEM('',(#5444),#3114);
#3550 = CARTESIAN_POINT ( 'NONE',  ( -0.6802310551622114954, 2.222614453595284090E-15, 47.14310755735262859 ) ) ;
#3551 = CARTESIAN_POINT ( 'NONE',  ( 31.14585677005056041, 25.00000000000018474, 398.7793066466517757 ) ) ;
#3552 = AXIS2_PLACEMENT_3D ( 'NONE', #3919, #145, #4758 ) ;
#3553 = CIRCLE ( 'NONE', #1440, 14.00000000000004086 ) ;
#3554 = EDGE_LOOP ( 'NONE', ( #947, #659, #3283, #1710 ) ) ;
#3555 = CARTESIAN_POINT ( 'NONE',  ( -105.2090356704102447, 25.00000000000018474, 560.1816718768288865 ) ) ;
#3556 = VERTEX_POINT ( 'NONE', #1720 ) ;
#3557 = AXIS2_PLACEMENT_3D ( 'NONE', #4391, #2273, #2328 ) ;
#3558 = LINE ( 'NONE', #3206, #464 ) ;
#3559 = CIRCLE ( 'NONE', #3122, 27.43532828739476415 ) ;
#3560 = ADVANCED_FACE ( 'NONE', ( #1283 ), #518, .F. ) ;
#3561 = COLOUR_RGB ( '',0.7921568627450980005, 0.8196078431372548767, 0.9333333333333333481 ) ;
#3562 = CARTESIAN_POINT ( 'NONE',  ( -108.3530091724271358, 15.00000000000001421, 123.8676211295743599 ) ) ;
#3563 = EDGE_CURVE ( 'NONE', #2642, #2780, #3484, .T. ) ;
#3564 = EDGE_CURVE ( 'NONE', #1930, #3639, #4691, .T. ) ;
#3565 = ORIENTED_EDGE ( 'NONE', *, *, #4623, .T. ) ;
#3566 = ADVANCED_FACE ( 'NONE', ( #1662 ), #2315, .T. ) ;
#3567 = EDGE_LOOP ( 'NONE', ( #4667, #4131 ) ) ;
#3568 = CARTESIAN_POINT ( 'NONE',  ( 151.9714219172562935, 84.45434506795673713, -11.99999999999995559 ) ) ;
#3569 = DIRECTION ( 'NONE',  ( 0.000000000000000000, 0.000000000000000000, -1.000000000000000000 ) ) ;
#3570 = DIRECTION ( 'NONE',  ( 5.551115123125772841E-17, -1.848892746611743135E-31, -1.000000000000000000 ) ) ;
#3571 = FACE_OUTER_BOUND ( 'NONE', #4807, .T. ) ;
#3572 = CARTESIAN_POINT ( 'NONE',  ( -86.02857808274413287, -21.54565493204320248, -12.00000000000001066 ) ) ;
#3573 = EDGE_LOOP ( 'NONE', ( #5384, #1971 ) ) ;
#3574 = CARTESIAN_POINT ( 'NONE',  ( -51.80562710762752232, 15.00000000000001421, 127.0899108387844336 ) ) ;
#3575 = DIRECTION ( 'NONE',  ( 0.09383933793885568253, -2.673190762809473730E-31, -0.9955873536034882676 ) ) ;
#3576 = CARTESIAN_POINT ( 'NONE',  ( 33.59898979596731294, 5.421010862427522170E-17, 384.0431050523496310 ) ) ;
#3577 = DIRECTION ( 'NONE',  ( 0.4205749795070158337, 0.9072577839912276954, 0.000000000000000000 ) ) ;
#3578 = LINE ( 'NONE', #1560, #1514 ) ;
#3579 = CARTESIAN_POINT ( 'NONE',  ( -347.9826081498995336, 2.222614453595284090E-15, 139.3632357185260560 ) ) ;
#3580 = ADVANCED_FACE ( 'NONE', ( #458 ), #2109, .F. ) ;
#3581 = CARTESIAN_POINT ( 'NONE',  ( 34.60640066538617532, 25.00000000000018474, 295.6817845355782879 ) ) ;
#3582 = DIRECTION ( 'NONE',  ( 0.9393298923196350403, 2.523234146875358956E-16, -0.3430150920801929848 ) ) ;
#3583 = CARTESIAN_POINT ( 'NONE',  ( 29.77542608467487995, -25.00000000000000355, 249.2409987768023711 ) ) ;
#3584 = ORIENTED_EDGE ( 'NONE', *, *, #725, .F. ) ;
#3585 = CARTESIAN_POINT ( 'NONE',  ( 8.821273309647297722, 3.740497495074990297E-15, 380.5076279642372015 ) ) ;
#3586 = ORIENTED_EDGE ( 'NONE', *, *, #3858, .F. ) ;
#3587 = CARTESIAN_POINT ( 'NONE',  ( 132.2270686671745068, 85.40608534173219368, -9.999999999999953815 ) ) ;
#3588 = CARTESIAN_POINT ( 'NONE',  ( -317.7315818134219398, 3.490243377570107522E-15, 122.1259097777134457 ) ) ;
#3589 = EDGE_LOOP ( 'NONE', ( #1886, #5016 ) ) ;
#3590 = UNCERTAINTY_MEASURE_WITH_UNIT (LENGTH_MEASURE( 1.000000000000000082E-05 ), #5203, 'distance_accuracy_value', 'NONE');
#3591 = ORIENTED_EDGE ( 'NONE', *, *, #798, .T. ) ;
#3592 = LINE ( 'NONE', #1467, #1254 ) ;
#3593 = CARTESIAN_POINT ( 'NONE',  ( 133.9714219172562650, 80.45434506795683660, -2.000000000000001776 ) ) ;
#3594 = AXIS2_PLACEMENT_3D ( 'NONE', #1148, #2862, #2004 ) ;
#3595 = CARTESIAN_POINT ( 'NONE',  ( -60.76122282208098824, 0.000000000000000000, 167.0961341013325523 ) ) ;
#3596 = FACE_OUTER_BOUND ( 'NONE', #5409, .T. ) ;
#3597 = ADVANCED_FACE ( 'NONE', ( #3358 ), #1313, .T. ) ;
#3598 = CARTESIAN_POINT ( 'NONE',  ( -81.77293133282584847, 75.50260479418152215, -11.99999999999995559 ) ) ;
#3599 = VERTEX_POINT ( 'NONE', #901 ) ;
#3600 = FILL_AREA_STYLE ('',( #1143 ) ) ;
#3601 = CARTESIAN_POINT ( 'NONE',  ( 0.000000000000000000, 0.000000000000000000, -50.00000000000000000 ) ) ;
#3602 = DIRECTION ( 'NONE',  ( 0.000000000000000000, 1.000000000000000000, 0.000000000000000000 ) ) ;
#3603 = CARTESIAN_POINT ( 'NONE',  ( -349.7655555707375470, 2.222614453595284090E-15, 158.2793954369922176 ) ) ;
#3604 = CARTESIAN_POINT ( 'NONE',  ( -347.9826081498995336, 2.222614453595284090E-15, 139.3632357185260560 ) ) ;
#3605 = CARTESIAN_POINT ( 'NONE',  ( -348.7799179161582970, -14.95948628165117178, 101.1196613272007738 ) ) ;
#3606 = CARTESIAN_POINT ( 'NONE',  ( 36.35777514575885760, 2.222614453595284090E-15, 354.7349908125909792 ) ) ;
#3607 = APPLICATION_PROTOCOL_DEFINITION ( 'draft international standard', 'automotive_design', 1998, #815 ) ;
#3608 = CARTESIAN_POINT ( 'NONE',  ( -13.17877320795229856, -25.00000000000000355, 47.33401081801169141 ) ) ;
#3609 = CARTESIAN_POINT ( 'NONE',  ( -30.63277980166695258, 0.000000000000000000, 527.1358351633697339 ) ) ;
#3610 = EDGE_LOOP ( 'NONE', ( #1223, #323, #602, #1237, #1292, #3616, #4219 ) ) ;
#3611 = CARTESIAN_POINT ( 'NONE',  ( -80.59222536594943165, 25.00000000000018474, 529.1597157429057461 ) ) ;
#3612 = EDGE_LOOP ( 'NONE', ( #875, #2262 ) ) ;
#3613 = CARTESIAN_POINT ( 'NONE',  ( -0.8482259245422840710, 2.276824562219559311E-15, 36.14439046289818691 ) ) ;
#3614 = LINE ( 'NONE', #2340, #28 ) ;
#3615 = EDGE_CURVE ( 'NONE', #4307, #4331, #3990, .T. ) ;
#3616 = ORIENTED_EDGE ( 'NONE', *, *, #1535, .T. ) ;
#3617 = ORIENTED_EDGE ( 'NONE', *, *, #2774, .F. ) ;
#3618 = LINE ( 'NONE', #1551, #382 ) ;
#3619 = DIRECTION ( 'NONE',  ( 0.09383933793885568253, -2.673190762809473730E-31, -0.9955873536034882676 ) ) ;
#3620 = DIRECTION ( 'NONE',  ( -0.9955873536034882676, 5.452307672560243681E-31, -0.09383933793885551600 ) ) ;
#3621 = LINE ( 'NONE', #1603, #1887 ) ;
#3622 = EDGE_LOOP ( 'NONE', ( #654, #1024, #4834, #1363 ) ) ;
#3623 = AXIS2_PLACEMENT_3D ( 'NONE', #3048, #4360, #587 ) ;
#3624 = DIRECTION ( 'NONE',  ( 5.551115123125772841E-17, -1.848892746611743354E-31, -1.000000000000000000 ) ) ;
#3625 = PLANE ( 'NONE',  #4341 ) ;
#3626 = CARTESIAN_POINT ( 'NONE',  ( -207.8397519515728504, 5.421010862427522170E-17, 541.5412455041541762 ) ) ;
#3627 = CYLINDRICAL_SURFACE ( 'NONE', #2506, 31.50000000000114397 ) ;
#3628 = CIRCLE ( 'NONE', #985, 5.250000000000004441 ) ;
#3629 = EDGE_CURVE ( 'NONE', #278, #3745, #1749, .T. ) ;
#3630 = CARTESIAN_POINT ( 'NONE',  ( -80.02857808274418971, -21.54565493204321669, -2.000000000000001776 ) ) ;
#3631 = EDGE_CURVE ( 'NONE', #1799, #783, #1087, .T. ) ;
#3632 = VECTOR ( 'NONE', #1758, 999.9999999999998863 ) ;
#3633 = LINE ( 'NONE', #243, #1737 ) ;
#3634 = CARTESIAN_POINT ( 'NONE',  ( -121.8424039467700055, 25.00000000000018474, 535.4314447305361000 ) ) ;
#3635 = ITEM_DEFINED_TRANSFORMATION ( 'NONE', 'NONE', #840,  #2926 ) ;
#3636 = CARTESIAN_POINT ( 'NONE',  ( 34.60640066538633874, 2.222614453595284090E-15, 295.6817845355787995 ) ) ;
#3637 = CARTESIAN_POINT ( 'NONE',  ( -367.0882437885061904, 2.222614453595284090E-15, 297.8351940652699454 ) ) ;
#3638 = AXIS2_PLACEMENT_3D ( 'NONE', #1892, #2275, #2734 ) ;
#3639 = VERTEX_POINT ( 'NONE', #849 ) ;
#3640 = CARTESIAN_POINT ( 'NONE',  ( -285.5643670724624599, 24.99999999999997158, 494.2304181244473966 ) ) ;
#3641 = ORIENTED_EDGE ( 'NONE', *, *, #3424, .F. ) ;
#3642 = CARTESIAN_POINT ( 'NONE',  ( -78.28422483266231779, -26.49739520581859153, -10.00000000000006395 ) ) ;
#3643 = MECHANICAL_DESIGN_GEOMETRIC_PRESENTATION_REPRESENTATION (  '', ( #1521 ), #4513 ) ;
#3644 = LINE ( 'NONE', #5306, #2847 ) ;
#3645 = CIRCLE ( 'NONE', #1344, 6.000000000000032863 ) ;
#3646 = ORIENTED_EDGE ( 'NONE', *, *, #2042, .F. ) ;
#3647 = UNCERTAINTY_MEASURE_WITH_UNIT (LENGTH_MEASURE( 1.000000000000000082E-05 ), #4930, 'distance_accuracy_value', 'NONE');
#3648 = VECTOR ( 'NONE', #4241, 1000.000000000000000 ) ;
#3649 = CIRCLE ( 'NONE', #1798, 5.250000000000018652 ) ;
#3650 = VERTEX_POINT ( 'NONE', #3026 ) ;
#3651 = DIRECTION ( 'NONE',  ( 5.551115123125772841E-17, -1.848892746611743135E-31, -1.000000000000000000 ) ) ;
#3652 = DIRECTION ( 'NONE',  ( 5.551115123125772841E-17, -1.848892746611743135E-31, -1.000000000000000000 ) ) ;
#3653 = CARTESIAN_POINT ( 'NONE',  ( 102.9433289385998478, 15.00000000000001421, 135.9081080810072137 ) ) ;
#3654 = PLANE ( 'NONE',  #4074 ) ;
#3655 = CIRCLE ( 'NONE', #131, 6.000000000000032863 ) ;
#3656 = DIRECTION ( 'NONE',  ( 3.204747427460360459E-31, -1.000000000000000000, 1.848892746611743354E-31 ) ) ;
#3657 = EDGE_LOOP ( 'NONE', ( #3508, #2954, #2173, #3087, #2017, #5072 ) ) ;
#3658 = DIRECTION ( 'NONE',  ( 5.551115123125772841E-17, -1.848892746611743135E-31, -1.000000000000000000 ) ) ;
#3659 = CARTESIAN_POINT ( 'NONE',  ( -367.0882437885061904, 2.222614453595284090E-15, 297.8351940652699454 ) ) ;
#3660 = PLANE ( 'NONE',  #2855 ) ;
#3661 = FACE_OUTER_BOUND ( 'NONE', #5413, .T. ) ;
#3662 = EDGE_CURVE ( 'NONE', #1126, #229, #1791, .T. ) ;
#3663 = CARTESIAN_POINT ( 'NONE',  ( -357.8553543223658835, 2.759321206427282701E-15, 37.98945711520877211 ) ) ;
#3664 = CARTESIAN_POINT ( 'NONE',  ( -207.8397519515722252, 24.99999999999997158, 541.5412455041529256 ) ) ;
#3665 = CARTESIAN_POINT ( 'NONE',  ( 33.59898979596731294, 5.421010862427522170E-17, 384.0431050523496310 ) ) ;
#3666 = EDGE_CURVE ( 'NONE', #405, #3533, #2501, .T. ) ;
#3667 = ADVANCED_FACE ( 'NONE', ( #1810 ), #3498, .F. ) ;
#3668 = ORIENTED_EDGE ( 'NONE', *, *, #3501, .F. ) ;
#3669 = CARTESIAN_POINT ( 'NONE',  ( -360.7307227603797060, 25.00000000000018474, 354.4373729494859049 ) ) ;
#3670 = VECTOR ( 'NONE', #5305, 1000.000000000000000 ) ;
#3671 = ORIENTED_EDGE ( 'NONE', *, *, #1674, .T. ) ;
#3672 = CARTESIAN_POINT ( 'NONE',  ( -319.3419943896644213, 2.222614453595281723E-15, 41.61954360114513207 ) ) ;
#3673 = EDGE_LOOP ( 'NONE', ( #4411, #3480, #4928 ) ) ;
#3674 = VERTEX_POINT ( 'NONE', #2637 ) ;
#3675 = DIRECTION ( 'NONE',  ( 5.551115123125772841E-17, -1.848892746611743135E-31, -1.000000000000000000 ) ) ;
#3676 = DIRECTION ( 'NONE',  ( -0.9955873536034882676, 5.502656983963329947E-31, -0.09383933793885568253 ) ) ;
#3677 = DIRECTION ( 'NONE',  ( -1.000000000000000000, -1.219242865862092731E-16, 0.000000000000000000 ) ) ;
#3678 = CARTESIAN_POINT ( 'NONE',  ( -80.02857808274404761, 80.45434506795689344, -9.999999999999841904 ) ) ;
#3679 = DIRECTION ( 'NONE',  ( 5.551115123125772841E-17, -1.848892746611743135E-31, -1.000000000000000000 ) ) ;
#3680 = VERTEX_POINT ( 'NONE', #3953 ) ;
#3681 = DIRECTION ( 'NONE',  ( 0.000000000000000000, 0.000000000000000000, 1.000000000000000000 ) ) ;
#3682 = CARTESIAN_POINT ( 'NONE',  ( -85.27857808274414708, 80.45434506795689344, -26.84924240491753977 ) ) ;
#3683 = CARTESIAN_POINT ( 'NONE',  ( 16.31778627263218695, 2.276824562219550240E-15, 46.88347912285639296 ) ) ;
#3684 = DIRECTION ( 'NONE',  ( -1.000000000000000000, 3.759415251443877379E-31, -5.551115123125772841E-17 ) ) ;
#3685 = LINE ( 'NONE', #1205, #3381 ) ;
#3686 = CARTESIAN_POINT ( 'NONE',  ( -334.2906958041451162, 24.99999999999997158, 430.9840019716597226 ) ) ;
#3687 = EDGE_CURVE ( 'NONE', #4708, #484, #4012, .T. ) ;
#3688 = CONTEXT_DEPENDENT_SHAPE_REPRESENTATION ( #5200, #873 ) ;
#3689 = CARTESIAN_POINT ( 'NONE',  ( -367.0882437885064746, -24.99999999999981881, 297.8351940652706276 ) ) ;
#3690 = ORIENTED_EDGE ( 'NONE', *, *, #78, .T. ) ;
#3691 = CARTESIAN_POINT ( 'NONE',  ( -223.9642223310802649, 24.99999999999997158, 534.3227077390027944 ) ) ;
#3692 = VERTEX_POINT ( 'NONE', #3055 ) ;
#3693 = DIRECTION ( 'NONE',  ( -0.09383933793885536334, 2.611561004589082183E-31, 0.9955873536034882676 ) ) ;
#3694 = SURFACE_SIDE_STYLE ('',( #2115 ) ) ;
#3695 = ORIENTED_EDGE ( 'NONE', *, *, #4226, .T. ) ;
#3696 = ORIENTED_EDGE ( 'NONE', *, *, #4133, .T. ) ;
#3697 = CYLINDRICAL_SURFACE ( 'NONE', #3895, 14.00000000000001243 ) ;
#3698 = DIRECTION ( 'NONE',  ( -0.9955873536034883786, 5.452307672560241053E-31, -0.09383933793885559926 ) ) ;
#3699 = CARTESIAN_POINT ( 'NONE',  ( 131.3198108831832656, 84.98551036222518462, -10.00000000000000888 ) ) ;
#3700 = CARTESIAN_POINT ( 'NONE',  ( 151.9714219172563219, 84.45434506795673713, 152.0000000000001990 ) ) ;
#3701 = CARTESIAN_POINT ( 'NONE',  ( 139.9714219172562935, 80.45434506795683660, -2.000000000000001332 ) ) ;
#3702 = VERTEX_POINT ( 'NONE', #4749 ) ;
#3703 = VERTEX_POINT ( 'NONE', #2732 ) ;
#3704 = DIRECTION ( 'NONE',  ( 0.09383933793885568253, -2.673190762809473730E-31, -0.9955873536034882676 ) ) ;
#3705 = CARTESIAN_POINT ( 'NONE',  ( -105.2090356704105147, 2.222614453595284090E-15, 560.1816718768288865 ) ) ;
#3706 = LINE ( 'NONE', #5373, #2413 ) ;
#3707 = DIRECTION ( 'NONE',  ( -1.000000000000000000, 0.000000000000000000, -7.228014483236656373E-17 ) ) ;
#3708 = CARTESIAN_POINT ( 'NONE',  ( -86.02857808274404761, 80.45434506795689344, -2.000000000000113243 ) ) ;
#3709 = CARTESIAN_POINT ( 'NONE',  ( -336.1069982926114221, 25.00000000000018474, 349.6877309229307684 ) ) ;
#3710 = CARTESIAN_POINT ( 'NONE',  ( 16.26935751051944479, 3.252606517456513302E-16, 140.3055424402290896 ) ) ;
#3711 = AXIS2_PLACEMENT_3D ( 'NONE', #5423, #4201, #43 ) ;
#3712 = ORIENTED_EDGE ( 'NONE', *, *, #1206, .F. ) ;
#3713 = EDGE_LOOP ( 'NONE', ( #2025, #1406 ) ) ;
#3714 = AXIS2_PLACEMENT_3D ( 'NONE', #2952, #3369, #33 ) ;
#3715 = CYLINDRICAL_SURFACE ( 'NONE', #830, 12.50000000000003197 ) ;
#3716 = AXIS2_PLACEMENT_3D ( 'NONE', #3425, #30, #1354 ) ;
#3717 = VECTOR ( 'NONE', #4437, 1000.000000000000000 ) ;
#3718 = EDGE_CURVE ( 'NONE', #1349, #4228, #2236, .T. ) ;
#3719 = VERTEX_POINT ( 'NONE', #5209 ) ;
#3720 = AXIS2_PLACEMENT_3D ( 'NONE', #977, #5174, #1415 ) ;
#3721 = EDGE_CURVE ( 'NONE', #3127, #979, #5132, .T. ) ;
#3722 = COLOUR_RGB ( '',0.7921568627450980005, 0.8196078431372548767, 0.9333333333333333481 ) ;
#3723 = DIRECTION ( 'NONE',  ( 0.000000000000000000, -1.000000000000000000, 0.000000000000000000 ) ) ;
#3724 = ADVANCED_FACE ( 'NONE', ( #1058 ), #3978, .T. ) ;
#3725 = DIRECTION ( 'NONE',  ( -1.000000000000000000, 0.000000000000000000, -7.228014483236656373E-17 ) ) ;
#3726 = CARTESIAN_POINT ( 'NONE',  ( -77.37696704867103392, 84.98551036222526989, -11.99999999999990052 ) ) ;
#3727 = ADVANCED_FACE ( 'NONE', ( #1400 ), #2294, .T. ) ;
#3728 = AXIS2_PLACEMENT_3D ( 'NONE', #3066, #4275, #3042 ) ;
#3729 = EDGE_CURVE ( 'NONE', #265, #1569, #241, .T. ) ;
#3730 = AXIS2_PLACEMENT_3D ( 'NONE', #3269, #3679, #5367 ) ;
#3731 = AXIS2_PLACEMENT_3D ( 'NONE', #4846, #672, #4122 ) ;
#3732 = EDGE_LOOP ( 'NONE', ( #4164, #2392 ) ) ;
#3733 = EDGE_CURVE ( 'NONE', #2554, #3745, #5039, .T. ) ;
#3734 = ORIENTED_EDGE ( 'NONE', *, *, #3261, .F. ) ;
#3735 = CARTESIAN_POINT ( 'NONE',  ( 139.9714219172562650, 80.45434506795683660, -12.00000000000001066 ) ) ;
#3736 = VECTOR ( 'NONE', #1714, 1000.000000000000114 ) ;
#3737 = CARTESIAN_POINT ( 'NONE',  ( -375.1735816981183689, 3.367778697655406295E-15, 134.7914792180005179 ) ) ;
#3738 = DIRECTION ( 'NONE',  ( 1.000000000000000000, 0.000000000000000000, 8.260587980841931384E-17 ) ) ;
#3739 = CIRCLE ( 'NONE', #1360, 27.50000000000126832 ) ;
#3740 = DIRECTION ( 'NONE',  ( 5.551115123125772841E-17, -1.848892746611743135E-31, -1.000000000000000000 ) ) ;
#3741 = PRODUCT_DEFINITION_FORMATION_WITH_SPECIFIED_SOURCE ( 'ANY', '', #1704, .NOT_KNOWN. ) ;
#3742 = DIRECTION ( 'NONE',  ( 0.9983803615885644689, 0.000000000000000000, 0.05689159511111529371 ) ) ;
#3743 = CARTESIAN_POINT ( 'NONE',  ( 4.992201166475890517, 1.572093150103981429E-15, 252.6216919286947586 ) ) ;
#3744 = CARTESIAN_POINT ( 'NONE',  ( 18.31346110193259946, -24.99999999999981881, 444.2932575970297648 ) ) ;
#3745 = VERTEX_POINT ( 'NONE', #158 ) ;
#3746 = EDGE_CURVE ( 'NONE', #496, #1327, #5389, .T. ) ;
#3747 = CARTESIAN_POINT ( 'NONE',  ( -353.4252897503525332, 0.000000000000000000, 197.1073022275279243 ) ) ;
#3748 = CARTESIAN_POINT ( 'NONE',  ( 128.7214219172562366, 80.45434506795679397, -12.00000000000001066 ) ) ;
#3749 = VERTEX_POINT ( 'NONE', #3523 ) ;
#3750 = EDGE_LOOP ( 'NONE', ( #359, #2569 ) ) ;
#3751 = DIRECTION ( 'NONE',  ( 5.551115123125772841E-17, -1.848892746611743135E-31, -1.000000000000000000 ) ) ;
#3752 = CARTESIAN_POINT ( 'NONE',  ( 135.9827310413679413, 0.000000000000000000, 131.6034880481681171 ) ) ;
#3753 = CARTESIAN_POINT ( 'NONE',  ( 29.23877717791900466, 0.000000000000000000, 117.0961341013326233 ) ) ;
#3754 = ADVANCED_FACE ( 'NONE', ( #3544 ), #3104, .T. ) ;
#3755 = DIRECTION ( 'NONE',  ( 0.9955873536034882676, -5.498529991225536465E-31, 0.09383933793885551600 ) ) ;
#3756 = ORIENTED_EDGE ( 'NONE', *, *, #2386, .T. ) ;
#3757 = ORIENTED_EDGE ( 'NONE', *, *, #2583, .T. ) ;
#3758 = DIRECTION ( 'NONE',  ( -0.09383933793885536334, 2.626968444144180070E-31, 0.9955873536034882676 ) ) ;
#3759 = CIRCLE ( 'NONE', #5414, 39.24395386344908587 ) ;
#3760 = CARTESIAN_POINT ( 'NONE',  ( 139.9714219172563219, 80.45434506795683660, -2.000000000000001332 ) ) ;
#3761 = DIRECTION ( 'NONE',  ( 2.523234146875361914E-16, 1.000000000000000000, 1.456973175402238023E-31 ) ) ;
#3762 = AXIS2_PLACEMENT_3D ( 'NONE', #1893, #4731, #4317 ) ;
#3763 = CARTESIAN_POINT ( 'NONE',  ( -249.5207023207451300, 1.843143693225357538E-15, 491.2832465756980014 ) ) ;
#3764 = CARTESIAN_POINT ( 'NONE',  ( -121.8424039466566313, 3.794707603699265519E-15, 535.4314447305365547 ) ) ;
#3765 = CARTESIAN_POINT ( 'NONE',  ( -77.37696704867103392, -26.07682022631158247, -10.00000000000000888 ) ) ;
#3766 = VERTEX_POINT ( 'NONE', #5180 ) ;
#3767 = CYLINDRICAL_SURFACE ( 'NONE', #1317, 17.00000000000009948 ) ;
#3768 = DIRECTION ( 'NONE',  ( -1.000000000000000000, 0.000000000000000000, 0.000000000000000000 ) ) ;
#3769 = VERTEX_POINT ( 'NONE', #4775 ) ;
#3770 = CARTESIAN_POINT ( 'NONE',  ( 133.9714219172562366, -21.54565493204319182, -12.00000000000006573 ) ) ;
#3771 = LINE ( 'NONE', #2487, #153 ) ;
#3772 = DIRECTION ( 'NONE',  ( 0.000000000000000000, 1.000000000000000000, 0.000000000000000000 ) ) ;
#3773 = DIRECTION ( 'NONE',  ( 0.000000000000000000, 0.000000000000000000, 1.000000000000000000 ) ) ;
#3774 = EDGE_LOOP ( 'NONE', ( #2703, #393, #1766, #3516, #5187, #4095, #3696, #2830 ) ) ;
#3775 = EDGE_LOOP ( 'NONE', ( #4357, #930, #4382, #688 ) ) ;
#3776 = FACE_OUTER_BOUND ( 'NONE', #1897, .T. ) ;
#3777 = DIRECTION ( 'NONE',  ( -1.000000000000000000, 0.000000000000000000, 0.000000000000000000 ) ) ;
#3778 = CARTESIAN_POINT ( 'NONE',  ( -344.4167133082243595, 2.222614453595284090E-15, 101.5309162815936048 ) ) ;
#3779 =( NAMED_UNIT ( * ) SI_UNIT ( $, .STERADIAN. ) SOLID_ANGLE_UNIT ( ) );
#3780 = DIRECTION ( 'NONE',  ( -0.9955873536034882676, 5.456801509096969733E-31, -0.09383933793885547436 ) ) ;
#3781 = CARTESIAN_POINT ( 'NONE',  ( -35.15684241565247703, 1.843143693225357538E-15, 493.9702760599520275 ) ) ;
#3782 = LINE ( 'NONE', #50, #3028 ) ;
#3783 = EDGE_CURVE ( 'NONE', #4918, #557, #543, .T. ) ;
#3784 = EDGE_CURVE ( 'NONE', #2195, #3205, #5127, .T. ) ;
#3785 = ORIENTED_EDGE ( 'NONE', *, *, #2482, .F. ) ;
#3786 = ORIENTED_EDGE ( 'NONE', *, *, #3416, .T. ) ;
#3787 = CARTESIAN_POINT ( 'NONE',  ( -319.4001412858301592, 4.060433389145185367E-15, 161.1414952441278956 ) ) ;
#3788 = PLANE ( 'NONE',  #2143 ) ;
#3789 = VECTOR ( 'NONE', #1967, 1000.000000000000000 ) ;
#3790 = ORIENTED_EDGE ( 'NONE', *, *, #85, .F. ) ;
#3791 = CARTESIAN_POINT ( 'NONE',  ( -325.1600333418735431, 2.222614453595298289E-15, 103.3459595245619198 ) ) ;
#3792 = CARTESIAN_POINT ( 'NONE',  ( 137.9714219172560945, -39.54565493204318471, -11.99999999999995559 ) ) ;
#3793 = CARTESIAN_POINT ( 'NONE',  ( -347.7949294740212736, 2.222614453595284090E-15, 137.3720610113191469 ) ) ;
#3794 = AXIS2_PLACEMENT_3D ( 'NONE', #1454, #4067, #5262 ) ;
#3795 = DIRECTION ( 'NONE',  ( 0.09383933793885568253, -2.673190762809473730E-31, -0.9955873536034882676 ) ) ;
#3796 = DIRECTION ( 'NONE',  ( 0.09383933793885537722, -2.626968444144180508E-31, -0.9955873536034883786 ) ) ;
#3797 = CYLINDRICAL_SURFACE ( 'NONE', #4950, 12.50000000000009237 ) ;
#3798 = VECTOR ( 'NONE', #3693, 1000.000000000000114 ) ;
#3799 = ADVANCED_FACE ( 'NONE', ( #3902 ), #1891, .F. ) ;
#3800 = AXIS2_PLACEMENT_3D ( 'NONE', #2564, #2159, #480 ) ;
#3801 = ORIENTED_EDGE ( 'NONE', *, *, #414, .T. ) ;
#3802 = VERTEX_POINT ( 'NONE', #4415 ) ;
#3803 = PRESENTATION_LAYER_ASSIGNMENT (  '', '', ( #2579 ) ) ;
#3804 = EDGE_CURVE ( 'NONE', #994, #1569, #919, .T. ) ;
#3805 = VERTEX_POINT ( 'NONE', #4905 ) ;
#3806 = DIRECTION ( 'NONE',  ( -1.219242865862094703E-16, 1.000000000000000000, -1.149200448409289593E-17 ) ) ;
#3807 = DIRECTION ( 'NONE',  ( 1.000000000000000000, 0.000000000000000000, 0.000000000000000000 ) ) ;
#3808 = ADVANCED_FACE ( 'NONE', ( #760 ), #4260, .F. ) ;
#3809 = LINE ( 'NONE', #44, #3736 ) ;
#3810 = AXIS2_PLACEMENT_3D ( 'NONE', #401, #2923, #839 ) ;
#3811 = AXIS2_PLACEMENT_3D ( 'NONE', #1167, #1729, #4900 ) ;
#3812 = CYLINDRICAL_SURFACE ( 'NONE', #3469, 31.50000000000125766 ) ;
#3813 = ORIENTED_EDGE ( 'NONE', *, *, #4780, .T. ) ;
#3814 = VECTOR ( 'NONE', #1318, 1000.000000000000000 ) ;
#3815 = AXIS2_PLACEMENT_3D ( 'NONE', #868, #2572, #3738 ) ;
#3816 = AXIS2_PLACEMENT_3D ( 'NONE', #1330, #948, #1414 ) ;
#3817 = CARTESIAN_POINT ( 'NONE',  ( -342.0244061588616091, 3.740497495074990297E-15, 297.0039604601894894 ) ) ;
#3818 = CARTESIAN_POINT ( 'NONE',  ( 10.82492224058167984, 3.740497495074990297E-15, 312.2165827548582229 ) ) ;
#3819 = DIRECTION ( 'NONE',  ( 5.551115123125772841E-17, -1.848892746611743135E-31, -1.000000000000000000 ) ) ;
#3820 = AXIS2_PLACEMENT_3D ( 'NONE', #4142, #7, #2898 ) ;
#3821 = EDGE_CURVE ( 'NONE', #3095, #1738, #4124, .T. ) ;
#3822 = ORIENTED_EDGE ( 'NONE', *, *, #365, .F. ) ;
#3823 = EDGE_CURVE ( 'NONE', #2116, #1846, #2415, .T. ) ;
#3824 = ORIENTED_EDGE ( 'NONE', *, *, #1034, .F. ) ;
#3825 = FACE_OUTER_BOUND ( 'NONE', #4240, .T. ) ;
#3826 =( NAMED_UNIT ( * ) PLANE_ANGLE_UNIT ( ) SI_UNIT ( $, .RADIAN. ) );
#3827 = EDGE_CURVE ( 'NONE', #3100, #3205, #3706, .T. ) ;
#3828 = CARTESIAN_POINT ( 'NONE',  ( -48.13570084519476211, 0.000000000000000000, 62.68703548022115513 ) ) ;
#3829 = ORIENTED_EDGE ( 'NONE', *, *, #5085, .F. ) ;
#3830 = FACE_OUTER_BOUND ( 'NONE', #4276, .T. ) ;
#3831 = CARTESIAN_POINT ( 'NONE',  ( 131.3198108831832371, 84.98551036222518462, -11.99999999999995559 ) ) ;
#3832 = CARTESIAN_POINT ( 'NONE',  ( -342.0244061588616091, -24.99999999999981881, 297.0039604601892620 ) ) ;
#3833 = CYLINDRICAL_SURFACE ( 'NONE', #3714, 14.00000000000001243 ) ;
#3834 = CARTESIAN_POINT ( 'NONE',  ( -317.6171938649919753, 5.957787190994850470E-15, 142.2253355256612508 ) ) ;
#3835 = VERTEX_POINT ( 'NONE', #700 ) ;
#3836 = ORIENTED_EDGE ( 'NONE', *, *, #2482, .T. ) ;
#3837 = ORIENTED_EDGE ( 'NONE', *, *, #3333, .F. ) ;
#3838 = LINE ( 'NONE', #2957, #2858 ) ;
#3839 = DIRECTION ( 'NONE',  ( 0.000000000000000000, 1.000000000000000000, 0.000000000000000000 ) ) ;
#3840 = DIRECTION ( 'NONE',  ( -0.9955873536034882676, 5.436595176548168253E-31, -0.09383933793885573804 ) ) ;
#3841 = CYLINDRICAL_SURFACE ( 'NONE', #2401, 6.000000000000032863 ) ;
#3842 = VERTEX_POINT ( 'NONE', #1146 ) ;
#3843 = CARTESIAN_POINT ( 'NONE',  ( -213.0979982360503584, 1.517883041479706208E-15, 511.7519955242227070 ) ) ;
#3844 = CARTESIAN_POINT ( 'NONE',  ( -68.63039925413373510, -24.99999999999981881, 524.1455590405155363 ) ) ;
#3845 = DIRECTION ( 'NONE',  ( -0.9955873536034882676, 5.502656983963321189E-31, -0.09383933793885568253 ) ) ;
#3846 = EDGE_LOOP ( 'NONE', ( #1716, #3341, #1082, #4495 ) ) ;
#3847 = ADVANCED_FACE ( 'NONE', ( #4150, #2857 ), #2769, .T. ) ;
#3848 = VERTEX_POINT ( 'NONE', #2445 ) ;
#3849 = DIRECTION ( 'NONE',  ( 0.01527226085271972227, 2.095411779493299033E-31, 0.9998833722232041143 ) ) ;
#3850 =( NAMED_UNIT ( * ) PLANE_ANGLE_UNIT ( ) SI_UNIT ( $, .RADIAN. ) );
#3851 = ORIENTED_EDGE ( 'NONE', *, *, #795, .F. ) ;
#3852 = CARTESIAN_POINT ( 'NONE',  ( -14.89480152442229688, 0.000000000000000000, 508.6517828409968729 ) ) ;
#3853 = ORIENTED_EDGE ( 'NONE', *, *, #1776, .F. ) ;
#3854 = LINE ( 'NONE', #4624, #1781 ) ;
#3855 = CARTESIAN_POINT ( 'NONE',  ( -39.32426838447570816, -24.99999999999981881, 499.4571537926179872 ) ) ;
#3856 = CARTESIAN_POINT ( 'NONE',  ( -57.28677601057280100, 3.252606517456513302E-16, 546.4981013186296650 ) ) ;
#3857 = CARTESIAN_POINT ( 'NONE',  ( -380.0165819072154818, 2.222614453595300261E-15, 175.5167213778050552 ) ) ;
#3858 = EDGE_CURVE ( 'NONE', #534, #179, #3655, .T. ) ;
#3859 = EDGE_LOOP ( 'NONE', ( #1153, #3444 ) ) ;
#3860 = EDGE_LOOP ( 'NONE', ( #5274, #2865 ) ) ;
#3861 = ORIENTED_EDGE ( 'NONE', *, *, #2435, .T. ) ;
#3862 = CARTESIAN_POINT ( 'NONE',  ( -84.02857808274400497, -39.54565493204319893, -11.99999999999984368 ) ) ;
#3863 = DIRECTION ( 'NONE',  ( -0.09383933793885568253, 2.673190762809473730E-31, 0.9955873536034882676 ) ) ;
#3864 = DIRECTION ( 'NONE',  ( 5.551115123125772841E-17, -1.848892746611743135E-31, -1.000000000000000000 ) ) ;
#3865 = PRESENTATION_STYLE_ASSIGNMENT (( #1715 ) ) ;
#3866 = ORIENTED_EDGE ( 'NONE', *, *, #13, .T. ) ;
#3867 = VECTOR ( 'NONE', #851, 1000.000000000000114 ) ;
#3868 = EDGE_CURVE ( 'NONE', #1042, #2670, #2471, .T. ) ;
#3869 = LINE ( 'NONE', #208, #4631 ) ;
#3870 = CARTESIAN_POINT ( 'NONE',  ( -268.5984117390374877, 3.740497495074990297E-15, 475.6392848759629715 ) ) ;
#3871 = CARTESIAN_POINT ( 'NONE',  ( 133.9714219172562366, 80.45434506795683660, -12.00000000000001066 ) ) ;
#3872 = ORIENTED_EDGE ( 'NONE', *, *, #1692, .F. ) ;
#3873 = ORIENTED_EDGE ( 'NONE', *, *, #1030, .F. ) ;
#3874 = CARTESIAN_POINT ( 'NONE',  ( -86.02857808274404761, 80.45434506795689344, -12.00000000000001066 ) ) ;
#3875 = VERTEX_POINT ( 'NONE', #2824 ) ;
#3876 = CARTESIAN_POINT ( 'NONE',  ( -122.4270646331731598, 3.252606517456513302E-16, 560.5113017241549187 ) ) ;
#3877 = AXIS2_PLACEMENT_3D ( 'NONE', #1396, #5173, #2218 ) ;
#3878 = CARTESIAN_POINT ( 'NONE',  ( -85.27857808274403340, 80.45434506795689344, -12.00000000000001066 ) ) ;
#3879 = CARTESIAN_POINT ( 'NONE',  ( 6.585909452865815084, -24.99999999999981881, 393.9228865916069253 ) ) ;
#3880 = CARTESIAN_POINT ( 'NONE',  ( 5.624351423727524946, 2.222614453595284090E-15, 474.0483466084679662 ) ) ;
#3881 = DIRECTION ( 'NONE',  ( 0.000000000000000000, -1.000000000000000000, 0.000000000000000000 ) ) ;
#3882 = AXIS2_PLACEMENT_3D ( 'NONE', #2977, #5394, #2488 ) ;
#3883 = ORIENTED_EDGE ( 'NONE', *, *, #2813, .T. ) ;
#3884 = ORIENTED_EDGE ( 'NONE', *, *, #334, .F. ) ;
#3885 = EDGE_CURVE ( 'NONE', #2041, #4435, #3120, .T. ) ;
#3886 = AXIS2_PLACEMENT_3D ( 'NONE', #3090, #2720, #3531 ) ;
#3887 = EDGE_CURVE ( 'NONE', #3127, #2337, #296, .T. ) ;
#3888 = ORIENTED_EDGE ( 'NONE', *, *, #1207, .F. ) ;
#3889 = FACE_OUTER_BOUND ( 'NONE', #1709, .T. ) ;
#3890 = EDGE_CURVE ( 'NONE', #3314, #3599, #4695, .T. ) ;
#3891 = CARTESIAN_POINT ( 'NONE',  ( -77.37696704867111919, -26.07682022631158247, -11.99999999999995559 ) ) ;
#3892 = CARTESIAN_POINT ( 'NONE',  ( 29.23877717791899755, 0.000000000000000000, 67.09613410133263756 ) ) ;
#3893 = EDGE_CURVE ( 'NONE', #5050, #4617, #481, .T. ) ;
#3894 = CIRCLE ( 'NONE', #2925, 4.382543221487789964 ) ;
#3895 = AXIS2_PLACEMENT_3D ( 'NONE', #3365, #2975, #2872 ) ;
#3896 = DIRECTION ( 'NONE',  ( -0.9955873536034882676, 5.498529991225538217E-31, -0.09383933793885536334 ) ) ;
#3897 = EDGE_LOOP ( 'NONE', ( #3734, #4221, #2490, #4894, #4548, #2037, #3313, #1598 ) ) ;
#3898 = AXIS2_PLACEMENT_3D ( 'NONE', #4545, #1263, #2039 ) ;
#3899 = DIRECTION ( 'NONE',  ( 0.09383933793885568253, -2.673190762809473730E-31, -0.9955873536034882676 ) ) ;
#3900 =( GEOMETRIC_REPRESENTATION_CONTEXT ( 3 ) GLOBAL_UNCERTAINTY_ASSIGNED_CONTEXT ( ( #4084 ) ) GLOBAL_UNIT_ASSIGNED_CONTEXT ( ( #2934, #4935, #3779 ) ) REPRESENTATION_CONTEXT ( 'NONE', 'WORKASPACE' ) );
#3901 = CARTESIAN_POINT ( 'NONE',  ( 5.624351423727524946, 2.222614453595284090E-15, 474.0483466084679662 ) ) ;
#3902 = FACE_OUTER_BOUND ( 'NONE', #4426, .T. ) ;
#3903 = VECTOR ( 'NONE', #4022, 1000.000000000000000 ) ;
#3904 = AXIS2_PLACEMENT_3D ( 'NONE', #4441, #670, #348 ) ;
#3905 = VERTEX_POINT ( 'NONE', #3274 ) ;
#3906 = CARTESIAN_POINT ( 'NONE',  ( -30.63277980166695258, 0.000000000000000000, 527.1358351633697339 ) ) ;
#3907 = VECTOR ( 'NONE', #5385, 1000.000000000000000 ) ;
#3908 = CARTESIAN_POINT ( 'NONE',  ( 42.32140464565708982, 1.507013218141296740, 181.5526868136130076 ) ) ;
#3909 = CIRCLE ( 'NONE', #1364, 1.000000000000000888 ) ;
#3910 = AXIS2_PLACEMENT_3D ( 'NONE', #3327, #811, #3016 ) ;
#3911 = AXIS2_PLACEMENT_3D ( 'NONE', #2264, #1741, #3071 ) ;
#3912 = ADVANCED_FACE ( 'NONE', ( #1495 ), #3627, .T. ) ;
#3913 = ORIENTED_EDGE ( 'NONE', *, *, #4993, .T. ) ;
#3914 = CARTESIAN_POINT ( 'NONE',  ( -156.9923520473269321, 0.000000000000000000, 556.8176423728721147 ) ) ;
#3915 = VERTEX_POINT ( 'NONE', #1976 ) ;
#3916 = ADVANCED_FACE ( 'NONE', ( #3191 ), #3660, .T. ) ;
#3917 = FACE_OUTER_BOUND ( 'NONE', #5307, .T. ) ;
#3918 = CARTESIAN_POINT ( 'NONE',  ( 132.2270686671743647, -26.49739520581860575, -9.999999999999953815 ) ) ;
#3919 = CARTESIAN_POINT ( 'NONE',  ( -84.02857808274410445, -25.54565493204318116, -11.99999999999995559 ) ) ;
#3920 = AXIS2_PLACEMENT_3D ( 'NONE', #5346, #3624, #5284 ) ;
#3921 = ORIENTED_EDGE ( 'NONE', *, *, #3890, .F. ) ;
#3922 = ORIENTED_EDGE ( 'NONE', *, *, #2274, .T. ) ;
#3923 = UNCERTAINTY_MEASURE_WITH_UNIT (LENGTH_MEASURE( 1.000000000000000082E-05 ), #5102, 'distance_accuracy_value', 'NONE');
#3924 = ORIENTED_EDGE ( 'NONE', *, *, #4630, .T. ) ;
#3925 = EDGE_CURVE ( 'NONE', #3848, #4918, #4516, .T. ) ;
#3926 = FACE_OUTER_BOUND ( 'NONE', #2728, .T. ) ;
#3927 = CARTESIAN_POINT ( 'NONE',  ( -376.2835570001519159, 2.222614453595300656E-15, 114.5982141321147196 ) ) ;
#3928 = CARTESIAN_POINT ( 'NONE',  ( -357.2727026058461206, 5.421010862427522170E-17, 237.9263837252718758 ) ) ;
#3929 = AXIS2_PLACEMENT_3D ( 'NONE', #824, #5357, #2067 ) ;
#3930 = EDGE_LOOP ( 'NONE', ( #2441, #2784, #4956, #2678 ) ) ;
#3931 = CYLINDRICAL_SURFACE ( 'NONE', #1726, 6.000000000000032863 ) ;
#3932 = CARTESIAN_POINT ( 'NONE',  ( -30.63277980166709114, -24.99999999999981881, 527.1358351633700750 ) ) ;
#3933 = CARTESIAN_POINT ( 'NONE',  ( -74.77857808274411866, 80.45434506795689344, -26.84924240491753977 ) ) ;
#3934 = CARTESIAN_POINT ( 'NONE',  ( 137.9714219172562650, 84.45434506795687923, -5.551115123125782702E-14 ) ) ;
#3935 = CARTESIAN_POINT ( 'NONE',  ( 36.66581985038869362, 3.252606517456513302E-16, 340.1662229844753256 ) ) ;
#3936 = CIRCLE ( 'NONE', #5063, 14.00000000000004086 ) ;
#3937 = ORIENTED_EDGE ( 'NONE', *, *, #130, .F. ) ;
#3938 = CARTESIAN_POINT ( 'NONE',  ( -14.89480152442222582, 25.00000000000018474, 508.6517828409982940 ) ) ;
#3939 = ORIENTED_EDGE ( 'NONE', *, *, #1635, .T. ) ;
#3940 = DIRECTION ( 'NONE',  ( 0.000000000000000000, 1.000000000000000000, 0.000000000000000000 ) ) ;
#3941 = DIRECTION ( 'NONE',  ( -0.9955873536034881566, 5.462637660443544243E-31, -0.09383933793885600172 ) ) ;
#3942 = CARTESIAN_POINT ( 'NONE',  ( -347.8887688119608015, 2.222614453595284090E-15, 138.3676483649225588 ) ) ;
#3943 = AXIS2_PLACEMENT_3D ( 'NONE', #16, #5069, #1311 ) ;
#3944 = EDGE_LOOP ( 'NONE', ( #3913, #5356 ) ) ;
#3945 = ORIENTED_EDGE ( 'NONE', *, *, #983, .F. ) ;
#3946 = PLANE ( 'NONE',  #3911 ) ;
#3947 = FACE_OUTER_BOUND ( 'NONE', #3417, .T. ) ;
#3948 = CARTESIAN_POINT ( 'NONE',  ( -366.9888585194556754, 2.222614453595296317E-15, 99.40337302301858813 ) ) ;
#3949 = CYLINDRICAL_SURFACE ( 'NONE', #2936, 5.250000000000004441 ) ;
#3950 = ORIENTED_EDGE ( 'NONE', *, *, #3083, .T. ) ;
#3951 = CARTESIAN_POINT ( 'NONE',  ( 131.3198108831832656, 84.98551036222518462, -10.00000000000000888 ) ) ;
#3952 = CARTESIAN_POINT ( 'NONE',  ( 34.60640066538617532, -24.99999999999981881, 295.6817845355782879 ) ) ;
#3953 = CARTESIAN_POINT ( 'NONE',  ( -339.2542556961718674, -2.870467298361735770E-14, 239.6247169981594141 ) ) ;
#3954 = DIRECTION ( 'NONE',  ( 5.551115123125772841E-17, -1.848892746611743135E-31, -1.000000000000000000 ) ) ;
#3955 = AXIS2_PLACEMENT_3D ( 'NONE', #1706, #3344, #5002 ) ;
#3956 = ADVANCED_FACE ( 'NONE', ( #3222 ), #4532, .F. ) ;
#3957 = CARTESIAN_POINT ( 'NONE',  ( -322.3869033466408496, 2.222614453595269101E-15, 160.8599772303116140 ) ) ;
#3958 = CARTESIAN_POINT ( 'NONE',  ( 18.31346110193232590, 2.222614453595284090E-15, 444.2932575970293101 ) ) ;
#3959 = EDGE_CURVE ( 'NONE', #4657, #167, #2384, .T. ) ;
#3960 = EDGE_CURVE ( 'NONE', #1072, #832, #1883, .T. ) ;
#3961 = EDGE_LOOP ( 'NONE', ( #3757, #1158 ) ) ;
#3962 = CARTESIAN_POINT ( 'NONE',  ( 16.26935751051944479, 3.252606517456513302E-16, 140.3055424402290896 ) ) ;
#3963 = ORIENTED_EDGE ( 'NONE', *, *, #2515, .F. ) ;
#3964 = FACE_OUTER_BOUND ( 'NONE', #3897, .T. ) ;
#3965 = DIRECTION ( 'NONE',  ( 0.000000000000000000, 1.000000000000000000, 0.000000000000000000 ) ) ;
#3966 = ORIENTED_EDGE ( 'NONE', *, *, #2518, .T. ) ;
#3967 = ORIENTED_EDGE ( 'NONE', *, *, #156, .T. ) ;
#3968 = PLANE ( 'NONE',  #2323 ) ;
#3969 = PLANE ( 'NONE',  #5374 ) ;
#3970 = CARTESIAN_POINT ( 'NONE',  ( 137.9714219172562366, 84.45434506795687923, -12.00000000000001066 ) ) ;
#3971 = SURFACE_STYLE_FILL_AREA ( #1936 ) ;
#3972 = ORIENTED_EDGE ( 'NONE', *, *, #2878, .F. ) ;
#3973 = CIRCLE ( 'NONE', #3101, 30.50000000000113332 ) ;
#3974 = EDGE_CURVE ( 'NONE', #4519, #2521, #1637, .T. ) ;
#3975 = SURFACE_SIDE_STYLE ('',( #5317 ) ) ;
#3976 = FACE_OUTER_BOUND ( 'NONE', #5383, .T. ) ;
#3977 = CARTESIAN_POINT ( 'NONE',  ( 35.78913469918423829, 0.000000000000000000, 310.6402212931345161 ) ) ;
#3978 = PLANE ( 'NONE',  #4608 ) ;
#3979 = VECTOR ( 'NONE', #662, 1000.000000000000000 ) ;
#3980 = AXIS2_PLACEMENT_3D ( 'NONE', #4979, #5392, #367 ) ;
#3981 = DIRECTION ( 'NONE',  ( 5.551115123125772841E-17, -1.848892746611743135E-31, -1.000000000000000000 ) ) ;
#3982 = CIRCLE ( 'NONE', #1612, 14.00000000000002665 ) ;
#3983 = PRESENTATION_LAYER_ASSIGNMENT (  '', '', ( #3549 ) ) ;
#3984 = VERTEX_POINT ( 'NONE', #5041 ) ;
#3985 = CARTESIAN_POINT ( 'NONE',  ( -264.1404626571534777, 2.222614453595284090E-15, 511.7445549721628595 ) ) ;
#3986 = APPLICATION_PROTOCOL_DEFINITION ( 'draft international standard', 'automotive_design', 1998, #2615 ) ;
#3987 = CARTESIAN_POINT ( 'NONE',  ( 16.26935751051938439, -25.00000000000000355, 140.3055424402287770 ) ) ;
#3988 =( GEOMETRIC_REPRESENTATION_CONTEXT ( 3 ) GLOBAL_UNCERTAINTY_ASSIGNED_CONTEXT ( ( #2372 ) ) GLOBAL_UNIT_ASSIGNED_CONTEXT ( ( #4402, #2311, #2836 ) ) REPRESENTATION_CONTEXT ( 'NONE', 'WORKASPACE' ) );
#3989 = EDGE_CURVE ( 'NONE', #4465, #2285, #2677, .T. ) ;
#3990 = CIRCLE ( 'NONE', #2755, 27.43532828739476415 ) ;
#3991 = ORIENTED_EDGE ( 'NONE', *, *, #3666, .T. ) ;
#3992 = CARTESIAN_POINT ( 'NONE',  ( 9.699276322990401766, 25.00000000000018474, 297.8714164406044915 ) ) ;
#3993 = ORIENTED_EDGE ( 'NONE', *, *, #4885, .F. ) ;
#3994 = ADVANCED_FACE ( 'NONE', ( #4610, #1681 ), #5091, .T. ) ;
#3995 = AXIS2_PLACEMENT_3D ( 'NONE', #1089, #1529, #1944 ) ;
#3996 = DIRECTION ( 'NONE',  ( -1.000000000000000000, -1.219242865862094703E-16, 0.000000000000000000 ) ) ;
#3997 = AXIS2_PLACEMENT_3D ( 'NONE', #4719, #2681, #2286 ) ;
#3998 = MECHANICAL_DESIGN_GEOMETRIC_PRESENTATION_REPRESENTATION (  '', ( #4778 ), #5131 ) ;
#3999 = SURFACE_STYLE_FILL_AREA ( #1155 ) ;
#4000 = EDGE_LOOP ( 'NONE', ( #3837, #2466, #3148, #1842 ) ) ;
#4001 = PRODUCT_DEFINITION_FORMATION_WITH_SPECIFIED_SOURCE ( 'ANY', '', #1136, .NOT_KNOWN. ) ;
#4002 = ORIENTED_EDGE ( 'NONE', *, *, #2182, .T. ) ;
#4003 = LINE ( 'NONE', #4027, #2133 ) ;
#4004 = CARTESIAN_POINT ( 'NONE',  ( -86.02857808274421814, -21.54565493204321669, -2.000000000000002220 ) ) ;
#4005 = LINE ( 'NONE', #3699, #1071 ) ;
#4006 = CARTESIAN_POINT ( 'NONE',  ( -351.7361816674535362, 5.421010862427522170E-17, 179.1867298626658283 ) ) ;
#4007 = DIRECTION ( 'NONE',  ( 5.551115123125772841E-17, -1.848892746611743135E-31, -1.000000000000000000 ) ) ;
#4008 = ORIENTED_EDGE ( 'NONE', *, *, #2981, .T. ) ;
#4009 = PLANE ( 'NONE',  #3920 ) ;
#4010 = CARTESIAN_POINT ( 'NONE',  ( -347.9826081498995336, 2.222614453595284090E-15, 139.3632357185260560 ) ) ;
#4011 = CARTESIAN_POINT ( 'NONE',  ( -19.78983854945498422, 2.222614453595284090E-15, 515.1268587725810448 ) ) ;
#4012 = LINE ( 'NONE', #1420, #827 ) ;
#4013 = FACE_OUTER_BOUND ( 'NONE', #141, .T. ) ;
#4014 = FACE_OUTER_BOUND ( 'NONE', #4400, .T. ) ;
#4015 = CARTESIAN_POINT ( 'NONE',  ( 16.26935751051944479, 3.252606517456513302E-16, 140.3055424402290896 ) ) ;
#4016 = DIRECTION ( 'NONE',  ( 1.000000000000000000, 0.000000000000000000, 0.000000000000000000 ) ) ;
#4017 = CARTESIAN_POINT ( 'NONE',  ( -198.3455225866217404, 1.517883041479706208E-15, 518.3576047634792303 ) ) ;
#4018 = EDGE_LOOP ( 'NONE', ( #747, #3144, #4896, #1100 ) ) ;
#4019 = CARTESIAN_POINT ( 'NONE',  ( -198.3455225866221667, 24.99999999999997158, 518.3576047634796851 ) ) ;
#4020 = ORIENTED_EDGE ( 'NONE', *, *, #129, .T. ) ;
#4021 = DIRECTION ( 'NONE',  ( 1.000000000000000000, 0.000000000000000000, 0.000000000000000000 ) ) ;
#4022 = DIRECTION ( 'NONE',  ( 0.000000000000000000, 1.000000000000000000, 0.000000000000000000 ) ) ;
#4023 = AXIS2_PLACEMENT_3D ( 'NONE', #2798, #1563, #677 ) ;
#4024 = SHAPE_REPRESENTATION ( 'Base Mounting Flange Control Box Bracket small', ( #2926 ), #724 ) ;
#4025 = ORIENTED_EDGE ( 'NONE', *, *, #3868, .T. ) ;
#4026 = ORIENTED_EDGE ( 'NONE', *, *, #531, .F. ) ;
#4027 = CARTESIAN_POINT ( 'NONE',  ( 131.3198108831832087, -26.07682022631159668, -10.00000000000000888 ) ) ;
#4028 = CARTESIAN_POINT ( 'NONE',  ( -353.3314504124138011, 0.000000000000000000, 196.1117148739250808 ) ) ;
#4029 = ADVANCED_FACE ( 'NONE', ( #4254 ), #1446, .F. ) ;
#4030 = DIRECTION ( 'NONE',  ( -1.000000000000000000, -3.125627884642856345E-17, -5.551115123125772841E-17 ) ) ;
#4031 = FACE_OUTER_BOUND ( 'NONE', #5134, .T. ) ;
#4032 = ADVANCED_FACE ( 'NONE', ( #2987 ), #4661, .F. ) ;
#4033 = CARTESIAN_POINT ( 'NONE',  ( -349.7655555707380017, 2.222614453595284090E-15, 158.2793954369929850 ) ) ;
#4034 = VERTEX_POINT ( 'NONE', #2495 ) ;
#4035 = CARTESIAN_POINT ( 'NONE',  ( -84.02857808274403340, 98.45434506795682239, -5.551115123125782702E-14 ) ) ;
#4036 = CARTESIAN_POINT ( 'NONE',  ( -66.30461487616335603, 0.000000000000000000, 161.8139267001887447 ) ) ;
#4037 = CARTESIAN_POINT ( 'NONE',  ( -84.02857808274410445, -25.54565493204318116, -11.99999999999995559 ) ) ;
#4038 = EDGE_CURVE ( 'NONE', #936, #3100, #394, .T. ) ;
#4039 = PLANE ( 'NONE',  #4291 ) ;
#4040 = CARTESIAN_POINT ( 'NONE',  ( -285.5643670724624599, 24.99999999999997158, 494.2304181244473966 ) ) ;
#4041 = APPLICATION_PROTOCOL_DEFINITION ( 'draft international standard', 'automotive_design', 1998, #4397 ) ;
#4042 = CARTESIAN_POINT ( 'NONE',  ( -30.63277980166709114, -24.99999999999981881, 527.1358351633700750 ) ) ;
#4043 = CARTESIAN_POINT ( 'NONE',  ( 31.14585677005082687, 2.222614453595284090E-15, 398.7793066466531968 ) ) ;
#4044 = ORIENTED_EDGE ( 'NONE', *, *, #1722, .F. ) ;
#4045 = CARTESIAN_POINT ( 'NONE',  ( -299.8611223228771792, 24.99999999999997158, 439.6443911606498887 ) ) ;
#4046 = AXIS2_PLACEMENT_3D ( 'NONE', #4652, #4958, #2514 ) ;
#4047 = ORIENTED_EDGE ( 'NONE', *, *, #2102, .T. ) ;
#4048 = DIRECTION ( 'NONE',  ( 1.000000000000000000, 0.000000000000000000, 0.000000000000000000 ) ) ;
#4049 = DIRECTION ( 'NONE',  ( -0.09383933793885536334, 2.611561004589082183E-31, 0.9955873536034882676 ) ) ;
#4050 = EDGE_CURVE ( 'NONE', #3984, #1903, #376, .T. ) ;
#4051 = ORIENTED_EDGE ( 'NONE', *, *, #1207, .T. ) ;
#4052 = ORIENTED_EDGE ( 'NONE', *, *, #2742, .T. ) ;
#4053 = CYLINDRICAL_SURFACE ( 'NONE', #5032, 21.00000000000124700 ) ;
#4054 = DIRECTION ( 'NONE',  ( -1.000000000000000000, 0.000000000000000000, -8.260587980841931384E-17 ) ) ;
#4055 = CARTESIAN_POINT ( 'NONE',  ( -334.2354697480813002, 14.95948628165116823, 40.21575531256979019 ) ) ;
#4056 = DIRECTION ( 'NONE',  ( -1.000000000000000000, 0.000000000000000000, 0.000000000000000000 ) ) ;
#4057 = EDGE_CURVE ( 'NONE', #1390, #3339, #2903, .T. ) ;
#4058 = EDGE_LOOP ( 'NONE', ( #2511, #1133 ) ) ;
#4059 = EDGE_CURVE ( 'NONE', #1654, #5098, #2590, .T. ) ;
#4060 = VECTOR ( 'NONE', #1004, 1000.000000000000000 ) ;
#4061 = ADVANCED_FACE ( 'NONE', ( #1279 ), #4582, .F. ) ;
#4062 =( NAMED_UNIT ( * ) SI_UNIT ( $, .STERADIAN. ) SOLID_ANGLE_UNIT ( ) );
#4063 = DIRECTION ( 'NONE',  ( -0.9955873536034882676, 5.498835694391114214E-31, -0.09383933793885536334 ) ) ;
#4064 = EDGE_CURVE ( 'NONE', #2337, #664, #4180, .T. ) ;
#4065 = CARTESIAN_POINT ( 'NONE',  ( -320.6447527397726276, 2.276824562219559311E-15, 453.8399743637901906 ) ) ;
#4066 = DIRECTION ( 'NONE',  ( -0.01527226085271972227, -2.080004339938201584E-31, -0.9998833722232041143 ) ) ;
#4067 = DIRECTION ( 'NONE',  ( -0.09383933793885568253, 2.673190762809473730E-31, 0.9955873536034882676 ) ) ;
#4068 = AXIS2_PLACEMENT_3D ( 'NONE', #2209, #477, #2155 ) ;
#4069 = DIRECTION ( 'NONE',  ( 0.9955873536034882676, -5.273458392682099492E-31, 0.09383933793885600172 ) ) ;
#4070 = AXIS2_PLACEMENT_3D ( 'NONE', #419, #31, #1192 ) ;
#4071 = CARTESIAN_POINT ( 'NONE',  ( -8.629236981538166873, 25.00000000000000355, 142.6115645898824198 ) ) ;
#4072 = CARTESIAN_POINT ( 'NONE',  ( -334.2906958041451162, -25.00000000000003197, 430.9840019716597226 ) ) ;
#4073 = LINE ( 'NONE', #705, #2744 ) ;
#4074 = AXIS2_PLACEMENT_3D ( 'NONE', #3678, #4524, #5314 ) ;
#4075 = CIRCLE ( 'NONE', #4944, 4.382543221487789076 ) ;
#4076 = ORIENTED_EDGE ( 'NONE', *, *, #2999, .F. ) ;
#4077 = CARTESIAN_POINT ( 'NONE',  ( 4.992201166475890517, 1.572093150103981429E-15, 252.6216919286947586 ) ) ;
#4078 = VERTEX_POINT ( 'NONE', #1658 ) ;
#4079 = DIRECTION ( 'NONE',  ( 0.9955873536034883786, -5.498529991225525955E-31, 0.09383933793885444741 ) ) ;
#4080 = CIRCLE ( 'NONE', #4598, 6.000000000000032863 ) ;
#4081 =( GEOMETRIC_REPRESENTATION_CONTEXT ( 3 ) GLOBAL_UNCERTAINTY_ASSIGNED_CONTEXT ( ( #3534 ) ) GLOBAL_UNIT_ASSIGNED_CONTEXT ( ( #2989, #151, #4662 ) ) REPRESENTATION_CONTEXT ( 'NONE', 'WORKASPACE' ) );
#4082 = AXIS2_PLACEMENT_3D ( 'NONE', #828, #1667, #2892 ) ;
#4083 = ORIENTED_EDGE ( 'NONE', *, *, #4812, .T. ) ;
#4084 = UNCERTAINTY_MEASURE_WITH_UNIT (LENGTH_MEASURE( 1.000000000000000082E-05 ), #2934, 'distance_accuracy_value', 'NONE');
#4085 = AXIS2_PLACEMENT_3D ( 'NONE', #2559, #4649, #781 ) ;
#4086 = CIRCLE ( 'NONE', #4604, 28.50000000000127542 ) ;
#4087 = ORIENTED_EDGE ( 'NONE', *, *, #57, .T. ) ;
#4088 = DIRECTION ( 'NONE',  ( -5.551115123125772841E-17, 1.848892746611743135E-31, 1.000000000000000000 ) ) ;
#4089 = DIRECTION ( 'NONE',  ( 0.09383933793885568253, -2.673190762809473730E-31, -0.9955873536034882676 ) ) ;
#4090 = CARTESIAN_POINT ( 'NONE',  ( 4.898587196589413026E-15, 80.00000000000000000, 40.00000000000000000 ) ) ;
#4091 = DIRECTION ( 'NONE',  ( 0.000000000000000000, 1.000000000000000000, 0.000000000000000000 ) ) ;
#4092 = VECTOR ( 'NONE', #5424, 1000.000000000000114 ) ;
#4093 = CIRCLE ( 'NONE', #3392, 5.250000000000018652 ) ;
#4094 = DIRECTION ( 'NONE',  ( -0.9955873536034882676, 5.273458392682099492E-31, -0.09383933793885600172 ) ) ;
#4095 = ORIENTED_EDGE ( 'NONE', *, *, #3887, .T. ) ;
#4096 = EDGE_CURVE ( 'NONE', #3490, #2943, #1532, .T. ) ;
#4097 = PRESENTATION_STYLE_ASSIGNMENT (( #726 ) ) ;
#4098 = CYLINDRICAL_SURFACE ( 'NONE', #3731, 6.000000000000032863 ) ;
#4099 = CARTESIAN_POINT ( 'NONE',  ( -347.8887688119603467, 2.222614453595284090E-15, 138.3676483649222178 ) ) ;
#4100 = DIRECTION ( 'NONE',  ( -0.9955873536034882676, 5.406119142139367196E-31, -0.09383933793885596009 ) ) ;
#4101 = VECTOR ( 'NONE', #4819, 1000.000000000000000 ) ;
#4102 = PRESENTATION_STYLE_ASSIGNMENT (( #1147 ) ) ;
#4103 = DIRECTION ( 'NONE',  ( 1.000000000000000000, 0.000000000000000000, 7.228014483236656373E-17 ) ) ;
#4104 = CARTESIAN_POINT ( 'NONE',  ( -5.157059352427092236, 25.00000000000018474, 435.5986320196304860 ) ) ;
#4105 = CARTESIAN_POINT ( 'NONE',  ( -122.4270646331731598, 3.252606517456513302E-16, 560.5113017241549187 ) ) ;
#4106 = ORIENTED_EDGE ( 'NONE', *, *, #2854, .T. ) ;
#4107 = CARTESIAN_POINT ( 'NONE',  ( -320.6447527397745034, 24.99999999999997158, 453.8399743637903612 ) ) ;
#4108 = AXIS2_PLACEMENT_3D ( 'NONE', #5332, #1546, #2014 ) ;
#4109 = EDGE_LOOP ( 'NONE', ( #2640, #2602, #3993, #1487 ) ) ;
#4110 = CARTESIAN_POINT ( 'NONE',  ( -365.9639710083354203, 1.530808498934204340E-15, 196.9298978568966163 ) ) ;
#4111 = DIRECTION ( 'NONE',  ( -0.09383933793885568253, 2.673190762809473730E-31, 0.9955873536034882676 ) ) ;
#4112 = ORIENTED_EDGE ( 'NONE', *, *, #1653, .T. ) ;
#4113 = EDGE_LOOP ( 'NONE', ( #74, #1512 ) ) ;
#4114 = DIRECTION ( 'NONE',  ( -0.4205749795070158337, -0.9072577839912276954, 0.000000000000000000 ) ) ;
#4115 = CARTESIAN_POINT ( 'NONE',  ( 29.23877717791899755, 15.00000000000001421, 67.09613410133263756 ) ) ;
#4116 = DIRECTION ( 'NONE',  ( 5.551115123125772841E-17, -1.848892746611743135E-31, -1.000000000000000000 ) ) ;
#4117 = DIRECTION ( 'NONE',  ( 5.551115123125772841E-17, -1.848892746611743135E-31, -1.000000000000000000 ) ) ;
#4118 = CIRCLE ( 'NONE', #1730, 30.50000000000113332 ) ;
#4119 = LINE ( 'NONE', #5076, #1353 ) ;
#4120 = EDGE_LOOP ( 'NONE', ( #1310, #2628 ) ) ;
#4121 = ORIENTED_EDGE ( 'NONE', *, *, #2042, .T. ) ;
#4122 = DIRECTION ( 'NONE',  ( -1.000000000000000000, 0.000000000000000000, -7.228014483236656373E-17 ) ) ;
#4123 = CARTESIAN_POINT ( 'NONE',  ( 11.65031622824785984, 2.276824562219551028E-15, 35.95348720223918804 ) ) ;
#4124 = LINE ( 'NONE', #353, #4349 ) ;
#4125 = CARTESIAN_POINT ( 'NONE',  ( 159.4907110033991273, 0.000000000000000000, 139.1303977902171596 ) ) ;
#4126 = CARTESIAN_POINT ( 'NONE',  ( -57.28677601057306390, 25.00000000000018474, 546.4981013186294376 ) ) ;
#4127 = CARTESIAN_POINT ( 'NONE',  ( -72.60637664584184847, 3.252606517456513302E-16, 552.9197695054128872 ) ) ;
#4128 = EDGE_CURVE ( 'NONE', #2924, #5171, #5304, .T. ) ;
#4129 = VERTEX_POINT ( 'NONE', #2131 ) ;
#4130 = CARTESIAN_POINT ( 'NONE',  ( -48.20943979673047863, 3.740497495074990297E-15, 509.2978244404888528 ) ) ;
#4131 = ORIENTED_EDGE ( 'NONE', *, *, #3084, .F. ) ;
#4132 = EDGE_CURVE ( 'NONE', #8, #2651, #3809, .T. ) ;
#4133 = EDGE_CURVE ( 'NONE', #2337, #850, #4430, .T. ) ;
#4134 = DIRECTION ( 'NONE',  ( -0.4205749795070158337, -0.9072577839912276954, 0.000000000000000000 ) ) ;
#4135 = EDGE_CURVE ( 'NONE', #4528, #265, #4265, .T. ) ;
#4136 = CARTESIAN_POINT ( 'NONE',  ( 0.000000000000000000, 80.00000000000000000, -40.00000000000000000 ) ) ;
#4137 = ORIENTED_EDGE ( 'NONE', *, *, #3088, .T. ) ;
#4138 = EDGE_LOOP ( 'NONE', ( #636, #4762 ) ) ;
#4139 = DIRECTION ( 'NONE',  ( 5.551115123125772841E-17, -1.848892746611743135E-31, -1.000000000000000000 ) ) ;
#4140 = CARTESIAN_POINT ( 'NONE',  ( 6.123233995736766085E-15, 0.000000000000000000, 50.00000000000000000 ) ) ;
#4141 = PLANE ( 'NONE',  #3882 ) ;
#4142 = CARTESIAN_POINT ( 'NONE',  ( 0.000000000000000000, 80.00000000000000000, 0.000000000000000000 ) ) ;
#4143 = AXIS2_PLACEMENT_3D ( 'NONE', #908, #2174, #958 ) ;
#4144 = AXIS2_PLACEMENT_3D ( 'NONE', #2113, #4670, #2556 ) ;
#4145 = CARTESIAN_POINT ( 'NONE',  ( -98.02857808274420393, -25.54565493204307813, 152.0000000000001990 ) ) ;
#4146 = ORIENTED_EDGE ( 'NONE', *, *, #3261, .T. ) ;
#4147 = ORIENTED_EDGE ( 'NONE', *, *, #4457, .F. ) ;
#4148 = CYLINDRICAL_SURFACE ( 'NONE', #37, 39.24395386344908587 ) ;
#4149 = CARTESIAN_POINT ( 'NONE',  ( -77.37696704867103392, 84.98551036222526989, -11.99999999999990052 ) ) ;
#4150 = FACE_OUTER_BOUND ( 'NONE', #4058, .T. ) ;
#4151 = EDGE_CURVE ( 'NONE', #5171, #1751, #3130, .T. ) ;
#4152 = DIRECTION ( 'NONE',  ( 5.551115123125772841E-17, -1.848892746611743135E-31, -1.000000000000000000 ) ) ;
#4153 = CARTESIAN_POINT ( 'NONE',  ( 4.992201166475890517, 1.572093150103981429E-15, 252.6216919286947586 ) ) ;
#4154 = CARTESIAN_POINT ( 'NONE',  ( -12.39202333278750601, 25.00000000000000355, 98.84296066633362443 ) ) ;
#4155 = CARTESIAN_POINT ( 'NONE',  ( -1.533280346156490337, 2.222614453595284090E-15, 488.4857301958385278 ) ) ;
#4156 = CIRCLE ( 'NONE', #896, 40.00000000000000000 ) ;
#4157 = ORIENTED_EDGE ( 'NONE', *, *, #4298, .F. ) ;
#4158 = AXIS2_PLACEMENT_3D ( 'NONE', #234, #1078, #1553 ) ;
#4159 = DIRECTION ( 'NONE',  ( -0.01527226085271972227, -2.080004339938201146E-31, -0.9998833722232041143 ) ) ;
#4160 = ADVANCED_FACE ( 'NONE', ( #4795 ), #1470, .T. ) ;
#4161 =( NAMED_UNIT ( * ) SI_UNIT ( $, .STERADIAN. ) SOLID_ANGLE_UNIT ( ) );
#4162 = VECTOR ( 'NONE', #3940, 1000.000000000000000 ) ;
#4163 = TOROIDAL_SURFACE ( 'NONE', #1782, 28.50000000000115463, 1.000000000000000000 ) ;
#4164 = ORIENTED_EDGE ( 'NONE', *, *, #4230, .F. ) ;
#4165 = EDGE_LOOP ( 'NONE', ( #4047, #5116 ) ) ;
#4166 = VECTOR ( 'NONE', #96, 1000.000000000000000 ) ;
#4167 = DIRECTION ( 'NONE',  ( -1.000000000000000000, 0.000000000000000000, 0.000000000000000000 ) ) ;
#4168 = FACE_OUTER_BOUND ( 'NONE', #708, .T. ) ;
#4169 = FACE_OUTER_BOUND ( 'NONE', #706, .T. ) ;
#4170 = FACE_OUTER_BOUND ( 'NONE', #4674, .T. ) ;
#4171 = PRESENTATION_LAYER_ASSIGNMENT (  '', '', ( #1085 ) ) ;
#4172 = AXIS2_PLACEMENT_3D ( 'NONE', #3871, #4264, #5097 ) ;
#4173 = ORIENTED_EDGE ( 'NONE', *, *, #2417, .T. ) ;
#4174 = ORIENTED_EDGE ( 'NONE', *, *, #3662, .T. ) ;
#4175 = AXIS2_PLACEMENT_3D ( 'NONE', #3747, #1593, #2038 ) ;
#4176 = DIRECTION ( 'NONE',  ( 0.09383933793885568253, -2.673190762809473730E-31, -0.9955873536034882676 ) ) ;
#4177 = AXIS2_PLACEMENT_3D ( 'NONE', #2930, #1227, #845 ) ;
#4178 = FACE_OUTER_BOUND ( 'NONE', #525, .T. ) ;
#4179 = ADVANCED_BREP_SHAPE_REPRESENTATION ( '', ( #3114, #2926 ), #1963 ) ;
#4180 = LINE ( 'NONE', #72, #2149 ) ;
#4181 = CIRCLE ( 'NONE', #1698, 49.99999999999996447 ) ;
#4182 = CARTESIAN_POINT ( 'NONE',  ( -0.4023372602957597799, 1.572093150103981429E-15, 421.4664991284013809 ) ) ;
#4183 = CARTESIAN_POINT ( 'NONE',  ( -0.4023372603089575006, -24.99999999999981881, 421.4664991283988229 ) ) ;
#4184 = DIRECTION ( 'NONE',  ( -5.551115123125772841E-17, 1.848892746611743135E-31, 1.000000000000000000 ) ) ;
#4185 = AXIS2_PLACEMENT_3D ( 'NONE', #1115, #4443, #3681 ) ;
#4186 = VERTEX_POINT ( 'NONE', #123 ) ;
#4187 = ADVANCED_FACE ( 'NONE', ( #1882 ), #2632, .F. ) ;
#4188 = DIRECTION ( 'NONE',  ( 0.000000000000000000, 0.000000000000000000, 1.000000000000000000 ) ) ;
#4189 = ORIENTED_EDGE ( 'NONE', *, *, #1033, .F. ) ;
#4190 = DIRECTION ( 'NONE',  ( 0.000000000000000000, 1.000000000000000000, 0.000000000000000000 ) ) ;
#4191 = DIRECTION ( 'NONE',  ( -0.09383933793885537722, 2.626968444144180508E-31, 0.9955873536034883786 ) ) ;
#4192 = FACE_BOUND ( 'NONE', #5196, .T. ) ;
#4193 = LINE ( 'NONE', #1672, #389 ) ;
#4194 = AXIS2_PLACEMENT_3D ( 'NONE', #3503, #1812, #1894 ) ;
#4195 = VERTEX_POINT ( 'NONE', #4361 ) ;
#4196 = ADVANCED_FACE ( 'NONE', ( #4816 ), #1005, .F. ) ;
#4197 = ORIENTED_EDGE ( 'NONE', *, *, #765, .T. ) ;
#4198 = DIRECTION ( 'NONE',  ( 6.938893903907233308E-17, 0.000000000000000000, 1.000000000000000000 ) ) ;
#4199 = EDGE_CURVE ( 'NONE', #4710, #1493, #2219, .T. ) ;
#4200 = CIRCLE ( 'NONE', #1562, 5.250000000000004441 ) ;
#4201 = DIRECTION ( 'NONE',  ( -0.09383933793885537722, 2.611561004589082621E-31, 0.9955873536034883786 ) ) ;
#4202 = DIRECTION ( 'NONE',  ( -0.9955873536034884896, 5.273458392682100368E-31, -0.09383933793885443353 ) ) ;
#4203 = FILL_AREA_STYLE_COLOUR ( '', #2054 ) ;
#4204 = AXIS2_PLACEMENT_3D ( 'NONE', #1811, #2033, #4586 ) ;
#4205 = DIRECTION ( 'NONE',  ( 0.000000000000000000, -1.000000000000000000, 0.000000000000000000 ) ) ;
#4206 = CARTESIAN_POINT ( 'NONE',  ( -35.15684241565268309, -24.99999999999981881, 493.9702760599490716 ) ) ;
#4207 = FACE_OUTER_BOUND ( 'NONE', #2634, .T. ) ;
#4208 = ORIENTED_EDGE ( 'NONE', *, *, #1156, .F. ) ;
#4209 = DIRECTION ( 'NONE',  ( -0.9955873536034882676, 5.406119142139367196E-31, -0.09383933793885596009 ) ) ;
#4210 =( NAMED_UNIT ( * ) PLANE_ANGLE_UNIT ( ) SI_UNIT ( $, .RADIAN. ) );
#4211 = DIRECTION ( 'NONE',  ( -5.551115123125772841E-17, 1.848892746611743135E-31, 1.000000000000000000 ) ) ;
#4212 = VERTEX_POINT ( 'NONE', #2708 ) ;
#4213 = CARTESIAN_POINT ( 'NONE',  ( 29.23877717791899755, 15.00000000000001421, 67.09613410133263756 ) ) ;
#4214 = CARTESIAN_POINT ( 'NONE',  ( 29.23877717791899400, 0.000000000000000000, 17.09613410133265532 ) ) ;
#4215 = CARTESIAN_POINT ( 'NONE',  ( -38.26122282208105219, 0.000000000000000000, 67.09613410133258071 ) ) ;
#4216 = DIRECTION ( 'NONE',  ( 4.476705744456277327E-17, 0.000000000000000000, 1.000000000000000000 ) ) ;
#4217 = CARTESIAN_POINT ( 'NONE',  ( 151.9714219172562650, -25.54565493204307813, -11.99999999999995559 ) ) ;
#4218 = VERTEX_POINT ( 'NONE', #2655 ) ;
#4219 = ORIENTED_EDGE ( 'NONE', *, *, #4885, .T. ) ;
#4220 = CIRCLE ( 'NONE', #3955, 31.50000000000120082 ) ;
#4221 = ORIENTED_EDGE ( 'NONE', *, *, #2344, .F. ) ;
#4222 = DIRECTION ( 'NONE',  ( -5.551115123125772841E-17, 1.848892746611743354E-31, 1.000000000000000000 ) ) ;
#4223 = CARTESIAN_POINT ( 'NONE',  ( -338.5986743560152377, 14.95948628165116823, 39.80450035817695209 ) ) ;
#4224 = DIRECTION ( 'NONE',  ( 0.000000000000000000, 0.000000000000000000, -1.000000000000000000 ) ) ;
#4225 = CIRCLE ( 'NONE', #4143, 4.382543221487789076 ) ;
#4226 = EDGE_CURVE ( 'NONE', #3842, #463, #488, .T. ) ;
#4227 = DIRECTION ( 'NONE',  ( 0.9955873536034882676, -5.475514420260265162E-31, 0.09383933793885552987 ) ) ;
#4228 = VERTEX_POINT ( 'NONE', #3098 ) ;
#4229 = EDGE_CURVE ( 'NONE', #1493, #556, #996, .T. ) ;
#4230 = EDGE_CURVE ( 'NONE', #342, #860, #2750, .T. ) ;
#4231 = DIRECTION ( 'NONE',  ( 0.09383933793885537722, -2.626968444144180508E-31, -0.9955873536034883786 ) ) ;
#4232 = CARTESIAN_POINT ( 'NONE',  ( 9.699276322990401766, -24.99999999999981881, 297.8714164406044915 ) ) ;
#4233 = CARTESIAN_POINT ( 'NONE',  ( -80.02857808274410445, -21.54565493204320248, -12.00000000000001066 ) ) ;
#4234 = ORIENTED_EDGE ( 'NONE', *, *, #4132, .T. ) ;
#4235 = TOROIDAL_SURFACE ( 'NONE', #2296, 23.00000000000115108, 2.000000000000000000 ) ;
#4236 = VERTEX_POINT ( 'NONE', #150 ) ;
#4237 = FACE_OUTER_BOUND ( 'NONE', #3713, .T. ) ;
#4238 = DIRECTION ( 'NONE',  ( 5.551115123125772841E-17, -1.848892746611743135E-31, -1.000000000000000000 ) ) ;
#4239 = CIRCLE ( 'NONE', #1861, 77.49999999999998579 ) ;
#4240 = EDGE_LOOP ( 'NONE', ( #523, #4251 ) ) ;
#4241 = DIRECTION ( 'NONE',  ( 2.523234146875361914E-16, 1.000000000000000000, 1.456973175402238023E-31 ) ) ;
#4242 = DIRECTION ( 'NONE',  ( 0.09383933793885568253, -2.673190762809473730E-31, -0.9955873536034882676 ) ) ;
#4243 = CARTESIAN_POINT ( 'NONE',  ( -52.92425795463013571, -24.99999999999981881, 513.6488213284161475 ) ) ;
#4244 = CIRCLE ( 'NONE', #291, 27.43532828739476415 ) ;
#4245 = DIRECTION ( 'NONE',  ( 5.551115123125772841E-17, -1.848892746611743135E-31, -1.000000000000000000 ) ) ;
#4246 = PLANE ( 'NONE',  #2153 ) ;
#4247 = CIRCLE ( 'NONE', #470, 1.000000000000000888 ) ;
#4248 = ORIENTED_EDGE ( 'NONE', *, *, #756, .F. ) ;
#4249 = ORIENTED_EDGE ( 'NONE', *, *, #3960, .F. ) ;
#4250 = VECTOR ( 'NONE', #1744, 1000.000000000000000 ) ;
#4251 = ORIENTED_EDGE ( 'NONE', *, *, #971, .T. ) ;
#4252 = FACE_BOUND ( 'NONE', #5100, .T. ) ;
#4253 = CYLINDRICAL_SURFACE ( 'NONE', #4406, 5.250000000000018652 ) ;
#4254 = FACE_OUTER_BOUND ( 'NONE', #3359, .T. ) ;
#4255 = CIRCLE ( 'NONE', #3112, 12.50000000000009237 ) ;
#4256 = B_SPLINE_CURVE_WITH_KNOTS ( 'NONE', 3,
 ( #248, #4757, #1503, #1922, #4713, #4452, #3006, #1819, #4859, #2363, #4043, #581, #2645, #3880, #3200, #942, #2599, #3609, #554, #274, #3856, #88, #4274, #1356, #4302, #3041, #2239, #504, #3512, #2625, #969, #1410, #997, #2211, #528, #3637, #2185, #115 ),
 .UNSPECIFIED., .F., .F.,
 ( 4, 2, 2, 2, 2, 2, 2, 2, 2, 2, 2, 2, 2, 2, 2, 2, 2, 2, 4 ),
 ( 0.000000000000000000, 0.1028767157186024211, 0.2057534314372048423, 0.2571917892965060459, 0.3086301471558072773, 0.3600685050151084532, 0.4115068628744096846, 0.4558387458985032614, 0.4780046874105500776, 0.5001706289225968938, 0.5231687412733679876, 0.5461668536241390814, 0.5921630783256812691, 0.6381593030272234568, 0.6841555277287657555, 0.7631166457965743444, 0.8420777638643828222, 0.9210388819321914111, 1.000000000000000000 ),
 .UNSPECIFIED. ) ;
#4257 = EDGE_CURVE ( 'NONE', #2427, #5300, #5216, .T. ) ;
#4258 = DIRECTION ( 'NONE',  ( 0.9955873536034882676, -5.498835694391114214E-31, 0.09383933793885514130 ) ) ;
#4259 = ORIENTED_EDGE ( 'NONE', *, *, #4654, .F. ) ;
#4260 = TOROIDAL_SURFACE ( 'NONE', #2420, 28.50000000000115818, 1.000000000000000000 ) ;
#4261 = AXIS2_PLACEMENT_3D ( 'NONE', #2522, #2099, #1634 ) ;
#4262 = CARTESIAN_POINT ( 'NONE',  ( -48.20943979673047863, 3.740497495074990297E-15, 509.2978244404888528 ) ) ;
#4263 = CARTESIAN_POINT ( 'NONE',  ( 8.821273309634928950, -24.99999999999981881, 380.5076279642381110 ) ) ;
#4264 = DIRECTION ( 'NONE',  ( 5.551115123125772841E-17, -1.848892746611743135E-31, -1.000000000000000000 ) ) ;
#4265 = CIRCLE ( 'NONE', #4683, 5.250000000000018652 ) ;
#4266 = ORIENTED_EDGE ( 'NONE', *, *, #1465, .F. ) ;
#4267 = EDGE_CURVE ( 'NONE', #4320, #276, #2861, .T. ) ;
#4268 = ORIENTED_EDGE ( 'NONE', *, *, #798, .F. ) ;
#4269 = DIRECTION ( 'NONE',  ( 0.09383933793885568253, -2.673190762809473730E-31, -0.9955873536034882676 ) ) ;
#4270 = ORIENTED_EDGE ( 'NONE', *, *, #5188, .T. ) ;
#4271 = LINE ( 'NONE', #2850, #1690 ) ;
#4272 = LINE ( 'NONE', #855, #1343 ) ;
#4273 = CARTESIAN_POINT ( 'NONE',  ( 11.35554381054933160, -24.99999999999981881, 353.5846600851155017 ) ) ;
#4274 = CARTESIAN_POINT ( 'NONE',  ( -80.60298687151650654, 2.222614453595284090E-15, 555.2885198911399129 ) ) ;
#4275 = DIRECTION ( 'NONE',  ( 0.09383933793885568253, -2.673190762809473730E-31, -0.9955873536034882676 ) ) ;
#4276 = EDGE_LOOP ( 'NONE', ( #257, #3046, #4579, #507 ) ) ;
#4277 = VERTEX_POINT ( 'NONE', #3493 ) ;
#4278 = ORIENTED_EDGE ( 'NONE', *, *, #5358, .F. ) ;
#4279 = DIRECTION ( 'NONE',  ( 0.09383933793885568253, -2.673190762809473730E-31, -0.9955873536034882676 ) ) ;
#4280 = DIRECTION ( 'NONE',  ( 1.000000000000000000, 0.000000000000000000, 0.000000000000000000 ) ) ;
#4281 = DIRECTION ( 'NONE',  ( 1.000000000000000000, 0.000000000000000000, 0.000000000000000000 ) ) ;
#4282 = DIRECTION ( 'NONE',  ( 5.551115123125772841E-17, -1.848892746611743135E-31, -1.000000000000000000 ) ) ;
#4283 = EDGE_LOOP ( 'NONE', ( #5248, #3712, #4590, #1361 ) ) ;
#4284 = AXIS2_PLACEMENT_3D ( 'NONE', #3102, #2711, #2688 ) ;
#4285 = DIRECTION ( 'NONE',  ( 0.000000000000000000, -1.000000000000000000, 0.000000000000000000 ) ) ;
#4286 = CARTESIAN_POINT ( 'NONE',  ( -5.157059352427092236, -24.99999999999981881, 435.5986320196304860 ) ) ;
#4287 = DIRECTION ( 'NONE',  ( -0.09383933793885537722, 2.626968444144180508E-31, 0.9955873536034883786 ) ) ;
#4288 = AXIS2_PLACEMENT_3D ( 'NONE', #105, #702, #5377 ) ;
#4289 = ORIENTED_EDGE ( 'NONE', *, *, #422, .T. ) ;
#4290 = ORIENTED_EDGE ( 'NONE', *, *, #3974, .F. ) ;
#4291 = AXIS2_PLACEMENT_3D ( 'NONE', #1980, #4501, #2449 ) ;
#4292 = LINE ( 'NONE', #415, #4312 ) ;
#4293 = ADVANCED_FACE ( 'NONE', ( #3571 ), #5230, .T. ) ;
#4294 = EDGE_CURVE ( 'NONE', #4195, #5106, #3982, .T. ) ;
#4295 = ORIENTED_EDGE ( 'NONE', *, *, #4457, .T. ) ;
#4296 = CARTESIAN_POINT ( 'NONE',  ( -36.58361131987991399, 0.000000000000000000, 532.6725316595221784 ) ) ;
#4297 = VERTEX_POINT ( 'NONE', #950 ) ;
#4298 = EDGE_CURVE ( 'NONE', #936, #2195, #1052, .T. ) ;
#4299 = EDGE_CURVE ( 'NONE', #4129, #911, #3049, .T. ) ;
#4300 = CARTESIAN_POINT ( 'NONE',  ( -98.02857808274420393, -25.54565493204309234, 5.551115123125782702E-14 ) ) ;
#4301 = CARTESIAN_POINT ( 'NONE',  ( -268.5984117390373171, -25.00000000000003197, 475.6392848759601293 ) ) ;
#4302 = CARTESIAN_POINT ( 'NONE',  ( -122.4270646331731598, 3.252606517456513302E-16, 560.5113017241549187 ) ) ;
#4303 = DIRECTION ( 'NONE',  ( -0.9955873536034883786, 5.430490990731020552E-31, -0.09383933793885548824 ) ) ;
#4304 = EDGE_CURVE ( 'NONE', #3802, #2756, #1850, .T. ) ;
#4305 = ORIENTED_EDGE ( 'NONE', *, *, #3890, .T. ) ;
#4306 = VERTEX_POINT ( 'NONE', #4385 ) ;
#4307 = VERTEX_POINT ( 'NONE', #288 ) ;
#4308 = DIRECTION ( 'NONE',  ( -0.09383933793885568253, 2.673190762809473730E-31, 0.9955873536034882676 ) ) ;
#4309 = DIRECTION ( 'NONE',  ( -0.9955873536034882676, 5.452307672560250687E-31, -0.09383933793885569641 ) ) ;
#4310 = DIRECTION ( 'NONE',  ( 0.000000000000000000, 1.000000000000000000, 0.000000000000000000 ) ) ;
#4311 = ORIENTED_EDGE ( 'NONE', *, *, #4862, .F. ) ;
#4312 = VECTOR ( 'NONE', #521, 1000.000000000000114 ) ;
#4313 = CARTESIAN_POINT ( 'NONE',  ( -338.5048350180761076, 2.276824562219559311E-15, 38.80891300457378890 ) ) ;
#4314 = CARTESIAN_POINT ( 'NONE',  ( -354.3266237013165778, -24.99999999999981881, 381.2801272015587983 ) ) ;
#4315 = DIRECTION ( 'NONE',  ( -5.551115123125772841E-17, 1.848892746611743135E-31, 1.000000000000000000 ) ) ;
#4316 = EDGE_CURVE ( 'NONE', #276, #4320, #2576, .T. ) ;
#4317 = DIRECTION ( 'NONE',  ( -0.9955873536034882676, 5.452307672560245432E-31, -0.09383933793885568253 ) ) ;
#4318 = CARTESIAN_POINT ( 'NONE',  ( -341.0742871682481905, -6.873162489031925530E-30, 199.2758813053679887 ) ) ;
#4319 =( NAMED_UNIT ( * ) PLANE_ANGLE_UNIT ( ) SI_UNIT ( $, .RADIAN. ) );
#4320 = VERTEX_POINT ( 'NONE', #5366 ) ;
#4321 = CARTESIAN_POINT ( 'NONE',  ( 29.77542608467487995, 25.00000000000000355, 249.2409987768023711 ) ) ;
#4322 = ADVANCED_FACE ( 'NONE', ( #3596 ), #347, .T. ) ;
#4323 = ORIENTED_EDGE ( 'NONE', *, *, #298, .T. ) ;
#4324 = CIRCLE ( 'NONE', #984, 27.50000000000126477 ) ;
#4325 = DIRECTION ( 'NONE',  ( -1.000000000000000000, -3.125627884642856345E-17, -5.551115123125772841E-17 ) ) ;
#4326 = DIRECTION ( 'NONE',  ( -1.000000000000000000, -1.219242865862094703E-16, 0.000000000000000000 ) ) ;
#4327 = DIRECTION ( 'NONE',  ( -2.523234146875361914E-16, -1.000000000000000000, -1.456973175402238023E-31 ) ) ;
#4328 = CIRCLE ( 'NONE', #104, 1.000000000000000888 ) ;
#4329 = VERTEX_POINT ( 'NONE', #1995 ) ;
#4330 = VERTEX_POINT ( 'NONE', #3296 ) ;
#4331 = VERTEX_POINT ( 'NONE', #236 ) ;
#4332 = CARTESIAN_POINT ( 'NONE',  ( -338.5986743560152377, 14.95948628165116823, 39.80450035817695209 ) ) ;
#4333 = DIRECTION ( 'NONE',  ( 0.09383933793885537722, -2.626968444144180508E-31, -0.9955873536034883786 ) ) ;
#4334 = CARTESIAN_POINT ( 'NONE',  ( -353.5191290882918338, 0.000000000000000000, 198.1028895811323025 ) ) ;
#4335 = SURFACE_SIDE_STYLE ('',( #127 ) ) ;
#4336 = EDGE_LOOP ( 'NONE', ( #1763, #3937, #1623, #2786 ) ) ;
#4337 = VECTOR ( 'NONE', #1927, 1000.000000000000000 ) ;
#4338 = PLANE ( 'NONE',  #4284 ) ;
#4339 = CARTESIAN_POINT ( 'NONE',  ( -30.63277980166695258, 0.000000000000000000, 527.1358351633697339 ) ) ;
#4340 = CARTESIAN_POINT ( 'NONE',  ( -60.76122282208098824, -14.99999999999998579, 167.0961341013325523 ) ) ;
#4341 = AXIS2_PLACEMENT_3D ( 'NONE', #3220, #3704, #4413 ) ;
#4342 = VECTOR ( 'NONE', #5074, 1000.000000000000114 ) ;
#4343 = CIRCLE ( 'NONE', #4951, 4.382543221487789964 ) ;
#4344 = AXIS2_PLACEMENT_3D ( 'NONE', #3303, #70, #1305 ) ;
#4345 = AXIS2_PLACEMENT_3D ( 'NONE', #1670, #4191, #1270 ) ;
#4346 = CARTESIAN_POINT ( 'NONE',  ( 137.9714219172561798, 98.45434506795687923, -5.551115123125782702E-14 ) ) ;
#4347 = CARTESIAN_POINT ( 'NONE',  ( -367.0460729392618759, 0.000000000000000000, 268.0688838304710089 ) ) ;
#4348 =( NAMED_UNIT ( * ) SI_UNIT ( $, .STERADIAN. ) SOLID_ANGLE_UNIT ( ) );
#4349 = VECTOR ( 'NONE', #1915, 1000.000000000000000 ) ;
#4350 = VERTEX_POINT ( 'NONE', #2320 ) ;
#4351 = CARTESIAN_POINT ( 'NONE',  ( 5.624351423727398824, 25.00000000000018474, 474.0483466084681368 ) ) ;
#4352 = ORIENTED_EDGE ( 'NONE', *, *, #3117, .T. ) ;
#4353 = CARTESIAN_POINT ( 'NONE',  ( 133.9714219172562366, 80.45434506795683660, -12.00000000000001066 ) ) ;
#4354 = PRODUCT_DEFINITION_FORMATION_WITH_SPECIFIED_SOURCE ( 'ANY', '', #835, .NOT_KNOWN. ) ;
#4355 = DIRECTION ( 'NONE',  ( -0.09383933793885568253, 2.673190762809473730E-31, 0.9955873536034882676 ) ) ;
#4356 = FACE_BOUND ( 'NONE', #1847, .T. ) ;
#4357 = ORIENTED_EDGE ( 'NONE', *, *, #2519, .T. ) ;
#4358 = EDGE_LOOP ( 'NONE', ( #119, #4730, #633, #3824 ) ) ;
#4359 = CARTESIAN_POINT ( 'NONE',  ( 0.000000000000000000, 80.00000000000000000, -40.00000000000000000 ) ) ;
#4360 = DIRECTION ( 'NONE',  ( -0.09383933793885568253, 2.673190762809473730E-31, 0.9955873536034882676 ) ) ;
#4361 = CARTESIAN_POINT ( 'NONE',  ( 137.9714219172561513, 98.45434506795689344, -12.00000000000006573 ) ) ;
#4362 = ORIENTED_EDGE ( 'NONE', *, *, #422, .F. ) ;
#4363 = EDGE_CURVE ( 'NONE', #2285, #800, #219, .T. ) ;
#4364 = ADVANCED_FACE ( 'NONE', ( #4409 ), #3654, .T. ) ;
#4365 = CARTESIAN_POINT ( 'NONE',  ( -78.28422483266214726, 85.40608534173227895, -12.00000000000001066 ) ) ;
#4366 = EDGE_CURVE ( 'NONE', #3530, #167, #669, .T. ) ;
#4367 = CARTESIAN_POINT ( 'NONE',  ( 34.60640066538633874, 2.222614453595284090E-15, 295.6817845355787995 ) ) ;
#4368 = CARTESIAN_POINT ( 'NONE',  ( 133.9714219172562650, 80.45434506795683660, -2.000000000000001776 ) ) ;
#4369 = LINE ( 'NONE', #3223, #1962 ) ;
#4370 = FACE_BOUND ( 'NONE', #4484, .T. ) ;
#4371 = CARTESIAN_POINT ( 'NONE',  ( 35.78913469918393275, 25.00000000000018474, 310.6402212931347435 ) ) ;
#4372 = DIRECTION ( 'NONE',  ( 1.000000000000000000, 0.000000000000000000, 0.000000000000000000 ) ) ;
#4373 = AXIS2_PLACEMENT_3D ( 'NONE', #3180, #2404, #4407 ) ;
#4374 = CLOSED_SHELL ( 'NONE', ( #1295, #5350, #300, #734, #3724, #1772, #1496, #1102, #1101, #2748 ) ) ;
#4375 = ORIENTED_EDGE ( 'NONE', *, *, #3331, .F. ) ;
#4376 = CARTESIAN_POINT ( 'NONE',  ( 5.624351423727524946, 2.222614453595284090E-15, 474.0483466084679662 ) ) ;
#4377 = EDGE_LOOP ( 'NONE', ( #4973, #2851, #39, #2263 ) ) ;
#4378 = DIRECTION ( 'NONE',  ( 0.05689159511111523820, 0.000000000000000000, -0.9983803615885644689 ) ) ;
#4379 = CARTESIAN_POINT ( 'NONE',  ( 29.23877717791895492, -14.99999999999998579, 117.0961341013325665 ) ) ;
#4380 = EDGE_CURVE ( 'NONE', #281, #2877, #117, .T. ) ;
#4381 = EDGE_LOOP ( 'NONE', ( #2455, #2164, #1627, #5163 ) ) ;
#4382 = ORIENTED_EDGE ( 'NONE', *, *, #1870, .F. ) ;
#4383 = CARTESIAN_POINT ( 'NONE',  ( -78.28422483266226095, -26.49739520581859153, -12.00000000000006573 ) ) ;
#4384 = DIRECTION ( 'NONE',  ( -0.01527226085271972227, -2.080004339938201146E-31, -0.9998833722232041143 ) ) ;
#4385 = CARTESIAN_POINT ( 'NONE',  ( -323.1537148033839344, 3.735172737399554547E-15, 200.9649893882672984 ) ) ;
#4386 = CARTESIAN_POINT ( 'NONE',  ( 29.23877717791895492, -14.99999999999998579, 67.09613410133256650 ) ) ;
#4387 = ORIENTED_EDGE ( 'NONE', *, *, #2540, .T. ) ;
#4388 = CARTESIAN_POINT ( 'NONE',  ( 139.2214219172562935, 80.45434506795679397, -2.000000000000001332 ) ) ;
#4389 = ADVANCED_FACE ( 'NONE', ( #4031 ), #1578, .F. ) ;
#4390 = CARTESIAN_POINT ( 'NONE',  ( -367.0882437885064746, -24.99999999999981881, 297.8351940652706276 ) ) ;
#4391 = CARTESIAN_POINT ( 'NONE',  ( 0.000000000000000000, 0.000000000000000000, 0.000000000000000000 ) ) ;
#4392 = CARTESIAN_POINT ( 'NONE',  ( -84.02857808274407603, 84.45434506795682239, -11.99999999999995559 ) ) ;
#4393 = EDGE_CURVE ( 'NONE', #2228, #2627, #3621, .T. ) ;
#4394 = FACE_OUTER_BOUND ( 'NONE', #4739, .T. ) ;
#4395 = CARTESIAN_POINT ( 'NONE',  ( 33.59898979596731294, 5.421010862427522170E-17, 384.0431050523496310 ) ) ;
#4396 = CARTESIAN_POINT ( 'NONE',  ( 10.82492224058160879, -24.99999999999981881, 312.2165827548579387 ) ) ;
#4397 = APPLICATION_CONTEXT ( 'automotive_design' ) ;
#4398 = ORIENTED_EDGE ( 'NONE', *, *, #4860, .F. ) ;
#4399 = CARTESIAN_POINT ( 'NONE',  ( -86.97194166595193110, 25.00000000000018474, 531.0655262460722952 ) ) ;
#4400 = EDGE_LOOP ( 'NONE', ( #2316, #1000, #435, #3924 ) ) ;
#4401 = DIRECTION ( 'NONE',  ( -1.000000000000000000, 2.523234146875361914E-16, -5.551115123125772841E-17 ) ) ;
#4402 =( LENGTH_UNIT ( ) NAMED_UNIT ( * ) SI_UNIT ( .MILLI., .METRE. ) );
#4403 = VERTEX_POINT ( 'NONE', #3268 ) ;
#4404 = VERTEX_POINT ( 'NONE', #1908 ) ;
#4405 = DIRECTION ( 'NONE',  ( -0.09383933793885537722, 2.626968444144180508E-31, 0.9955873536034883786 ) ) ;
#4406 = AXIS2_PLACEMENT_3D ( 'NONE', #5402, #5090, #1331 ) ;
#4407 = DIRECTION ( 'NONE',  ( -0.9955873536034882676, 5.452307672560245432E-31, -0.09383933793885568253 ) ) ;
#4408 = DIRECTION ( 'NONE',  ( -0.000000000000000000, -1.000000000000000000, -0.000000000000000000 ) ) ;
#4409 = FACE_OUTER_BOUND ( 'NONE', #4663, .T. ) ;
#4410 = DIRECTION ( 'NONE',  ( 1.000000000000000000, 0.000000000000000000, 0.000000000000000000 ) ) ;
#4411 = ORIENTED_EDGE ( 'NONE', *, *, #5428, .F. ) ;
#4412 = CIRCLE ( 'NONE', #4158, 14.00000000000002665 ) ;
#4413 = DIRECTION ( 'NONE',  ( -0.9955873536034882676, 5.452307672560245432E-31, -0.09383933793885568253 ) ) ;
#4414 = CARTESIAN_POINT ( 'NONE',  ( -80.60298687151718866, -24.99999999999981881, 555.2885198911441194 ) ) ;
#4415 = CARTESIAN_POINT ( 'NONE',  ( -38.26122282208105219, -14.99999999999998579, 67.09613410133258071 ) ) ;
#4416 = VECTOR ( 'NONE', #242, 1000.000000000000000 ) ;
#4417 = CIRCLE ( 'NONE', #2049, 31.50000000000125766 ) ;
#4418 = DIRECTION ( 'NONE',  ( 1.000000000000000000, 0.000000000000000000, 0.000000000000000000 ) ) ;
#4419 = AXIS2_PLACEMENT_3D ( 'NONE', #4767, #537, #1805 ) ;
#4420 = MECHANICAL_DESIGN_GEOMETRIC_PRESENTATION_REPRESENTATION (  '', ( #3549 ), #3900 ) ;
#4421 = DIRECTION ( 'NONE',  ( -1.219242865862094703E-16, 1.000000000000000000, -1.149200448409285278E-17 ) ) ;
#4422 = CARTESIAN_POINT ( 'NONE',  ( -207.8397519515728504, 5.421010862427522170E-17, 541.5412455041541762 ) ) ;
#4423 = PRODUCT_CONTEXT ( 'NONE', #1756, 'mechanical' ) ;
#4424 = CARTESIAN_POINT ( 'NONE',  ( 36.66581985038887126, -24.99999999999981881, 340.1662229844756098 ) ) ;
#4425 = CIRCLE ( 'NONE', #4771, 50.00000000000000000 ) ;
#4426 = EDGE_LOOP ( 'NONE', ( #991, #3972, #5225, #1197 ) ) ;
#4427 = CARTESIAN_POINT ( 'NONE',  ( -5.157059352426552223, 3.740497495074990297E-15, 435.5986320196309975 ) ) ;
#4428 = ORIENTED_EDGE ( 'NONE', *, *, #1935, .F. ) ;
#4429 = ADVANCED_FACE ( 'NONE', ( #1166 ), #4960, .T. ) ;
#4430 = CIRCLE ( 'NONE', #1092, 14.00000000000002665 ) ;
#4431 = DIRECTION ( 'NONE',  ( 0.9983803615885645799, 0.000000000000000000, 0.05689159511111524514 ) ) ;
#4432 = ADVANCED_BREP_SHAPE_REPRESENTATION ( '', ( #1341, #3192, #2926 ), #574 ) ;
#4433 = CIRCLE ( 'NONE', #2063, 21.00000000000124700 ) ;
#4434 = LINE ( 'NONE', #2429, #4337 ) ;
#4435 = VERTEX_POINT ( 'NONE', #4493 ) ;
#4436 = ORIENTED_EDGE ( 'NONE', *, *, #3397, .F. ) ;
#4437 = DIRECTION ( 'NONE',  ( -1.000000000000000000, -3.125627884642856345E-17, -5.551115123125772841E-17 ) ) ;
#4438 = CARTESIAN_POINT ( 'NONE',  ( -0.6802310551622114954, 2.222614453595284090E-15, 47.14310755735262859 ) ) ;
#4439 = FACE_OUTER_BOUND ( 'NONE', #3930, .T. ) ;
#4440 = CARTESIAN_POINT ( 'NONE',  ( -98.02857808274411866, 84.45434506795672291, -12.00000000000001066 ) ) ;
#4441 = CARTESIAN_POINT ( 'NONE',  ( 133.9714219172562650, 80.45434506795683660, -2.000000000000001776 ) ) ;
#4442 = ORIENTED_EDGE ( 'NONE', *, *, #224, .T. ) ;
#4443 = DIRECTION ( 'NONE',  ( 0.000000000000000000, 1.000000000000000000, 0.000000000000000000 ) ) ;
#4444 = CYLINDRICAL_SURFACE ( 'NONE', #5151, 4.382543221487789964 ) ;
#4445 = CYLINDRICAL_SURFACE ( 'NONE', #1243, 31.50000000000114397 ) ;
#4446 = DIRECTION ( 'NONE',  ( 0.000000000000000000, 1.000000000000000000, 0.000000000000000000 ) ) ;
#4447 = DIRECTION ( 'NONE',  ( 5.551115123125772841E-17, -1.848892746611743135E-31, -1.000000000000000000 ) ) ;
#4448 = CARTESIAN_POINT ( 'NONE',  ( -346.0119820531829191, 0.000000000000000000, 118.4559012928527721 ) ) ;
#4449 = CARTESIAN_POINT ( 'NONE',  ( -0.4023372602832280820, 25.00000000000018474, 421.4664991283991640 ) ) ;
#4450 = ITEM_DEFINED_TRANSFORMATION ( 'NONE', 'NONE', #2770,  #2926 ) ;
#4451 = CARTESIAN_POINT ( 'NONE',  ( -122.4270646331732451, -24.99999999999981881, 560.5113017241552598 ) ) ;
#4452 = CARTESIAN_POINT ( 'NONE',  ( 34.60640066538633874, 2.222614453595284090E-15, 295.6817845355787995 ) ) ;
#4453 = ORIENTED_EDGE ( 'NONE', *, *, #2737, .F. ) ;
#4454 = CARTESIAN_POINT ( 'NONE',  ( -174.3534642324312358, 25.00000000000018474, 552.7876087698487027 ) ) ;
#4455 = ORIENTED_EDGE ( 'NONE', *, *, #111, .F. ) ;
#4456 = CYLINDRICAL_SURFACE ( 'NONE', #3195, 5.250000000000018652 ) ;
#4457 = EDGE_CURVE ( 'NONE', #1678, #484, #4768, .T. ) ;
#4458 = CARTESIAN_POINT ( 'NONE',  ( -372.5496767551892958, 2.625968386833887277E-15, 176.2205164123462282 ) ) ;
#4459 = ADVANCED_FACE ( 'NONE', ( #753, #719 ), #4840, .F. ) ;
#4460 = EDGE_CURVE ( 'NONE', #249, #3236, #24, .T. ) ;
#4461 = CLOSED_SHELL ( 'NONE', ( #3500, #1717, #3727, #882 ) ) ;
#4462 = EDGE_LOOP ( 'NONE', ( #1961, #4888, #3883 ) ) ;
#4463 = UNCERTAINTY_MEASURE_WITH_UNIT (LENGTH_MEASURE( 1.000000000000000082E-05 ), #2821, 'distance_accuracy_value', 'NONE');
#4464 = ADVANCED_FACE ( 'NONE', ( #2760 ), #5279, .F. ) ;
#4465 = VERTEX_POINT ( 'NONE', #1934 ) ;
#4466 = DIRECTION ( 'NONE',  ( -1.000000000000000000, -1.219242865862094703E-16, 0.000000000000000000 ) ) ;
#4467 = CARTESIAN_POINT ( 'NONE',  ( -80.02857808274418971, -21.54565493204321669, -2.000000000000001776 ) ) ;
#4468 = DIRECTION ( 'NONE',  ( -3.125627884642856345E-17, 1.000000000000000000, 1.602373713730180668E-31 ) ) ;
#4469 = DIRECTION ( 'NONE',  ( -1.000000000000000000, 3.759415251443877379E-31, -5.551115123125772841E-17 ) ) ;
#4470 = CARTESIAN_POINT ( 'NONE',  ( -334.2354697480813002, 14.95948628165116823, 40.21575531256979019 ) ) ;
#4471 = ORIENTED_EDGE ( 'NONE', *, *, #4096, .F. ) ;
#4472 =( NAMED_UNIT ( * ) SI_UNIT ( $, .STERADIAN. ) SOLID_ANGLE_UNIT ( ) );
#4473 = FACE_OUTER_BOUND ( 'NONE', #4018, .T. ) ;
#4474 = DIRECTION ( 'NONE',  ( -0.09383933793885568253, 2.673190762809473730E-31, 0.9955873536034882676 ) ) ;
#4475 = DIRECTION ( 'NONE',  ( 1.000000000000000000, -3.759415251443877379E-31, 5.551115123125772841E-17 ) ) ;
#4476 = LINE ( 'NONE', #4802, #196 ) ;
#4477 = CARTESIAN_POINT ( 'NONE',  ( -351.6423423295148041, 5.421010862427522170E-17, 178.1911425090623311 ) ) ;
#4478 = CARTESIAN_POINT ( 'NONE',  ( -48.20943979671786650, 25.00000000000018474, 509.2978244404892507 ) ) ;
#4479 = CARTESIAN_POINT ( 'NONE',  ( -36.58361131987991399, 0.000000000000000000, 532.6725316595221784 ) ) ;
#4480 = CARTESIAN_POINT ( 'NONE',  ( 137.9714219172562366, -25.54565493204319182, -5.551115123125782702E-14 ) ) ;
#4481 = ORIENTED_EDGE ( 'NONE', *, *, #3430, .T. ) ;
#4482 = CARTESIAN_POINT ( 'NONE',  ( -12.39202333278749357, 1.572093150103981429E-15, 98.84296066633379496 ) ) ;
#4483 = AXIS2_PLACEMENT_3D ( 'NONE', #5364, #2044, #398 ) ;
#4484 = EDGE_LOOP ( 'NONE', ( #4052, #4508 ) ) ;
#4485 = CARTESIAN_POINT ( 'NONE',  ( 4.898587196589413815E-15, 80.00000000000000000, 40.00000000000000000 ) ) ;
#4486 = PRESENTATION_STYLE_ASSIGNMENT (( #4893 ) ) ;
#4487 = ADVANCED_FACE ( 'NONE', ( #1520 ), #694, .T. ) ;
#4488 = VERTEX_POINT ( 'NONE', #780 ) ;
#4489 = EDGE_LOOP ( 'NONE', ( #238, #4147 ) ) ;
#4490 = DIRECTION ( 'NONE',  ( 5.551115123125772841E-17, -1.848892746611743135E-31, -1.000000000000000000 ) ) ;
#4491 = CARTESIAN_POINT ( 'NONE',  ( 135.7157751673381085, 75.50260479418143689, -11.99999999999995559 ) ) ;
#4492 = CARTESIAN_POINT ( 'NONE',  ( -349.7655555707380017, 2.222614453595284090E-15, 158.2793954369929850 ) ) ;
#4493 = CARTESIAN_POINT ( 'NONE',  ( -321.3913159930368693, 5.712857831165385696E-15, 160.9538165682496640 ) ) ;
#4494 = DIRECTION ( 'NONE',  ( -0.9955873536034882676, 0.000000000000000000, -0.09383933793885600172 ) ) ;
#4495 = ORIENTED_EDGE ( 'NONE', *, *, #3821, .F. ) ;
#4496 = FACE_OUTER_BOUND ( 'NONE', #1466, .T. ) ;
#4497 = CARTESIAN_POINT ( 'NONE',  ( -334.2906958041416488, 0.000000000000000000, 430.9840019716568804 ) ) ;
#4498 = DIRECTION ( 'NONE',  ( 0.09383933793885537722, -2.626968444144180508E-31, -0.9955873536034883786 ) ) ;
#4499 = VECTOR ( 'NONE', #1907, 1000.000000000000000 ) ;
#4500 = AXIS2_PLACEMENT_3D ( 'NONE', #502, #5140, #1385 ) ;
#4501 = DIRECTION ( 'NONE',  ( -0.9072577839912278064, 0.4205749795070158892, 5.551115123125773458E-17 ) ) ;
#4502 = CARTESIAN_POINT ( 'NONE',  ( -23.53079058812344471, 25.00000000000018474, 476.4235034963351154 ) ) ;
#4503 = CARTESIAN_POINT ( 'NONE',  ( -364.1439395362590403, -24.99999999999981881, 237.2787335496889227 ) ) ;
#4504 = AXIS2_PLACEMENT_3D ( 'NONE', #709, #1188, #2396 ) ;
#4505 = PRODUCT_DEFINITION ( 'UNKNOWN', '', #4354, #5337 ) ;
#4506 = CIRCLE ( 'NONE', #2840, 5.250000000000004441 ) ;
#4507 =( GEOMETRIC_REPRESENTATION_CONTEXT ( 3 ) GLOBAL_UNCERTAINTY_ASSIGNED_CONTEXT ( ( #1549 ) ) GLOBAL_UNIT_ASSIGNED_CONTEXT ( ( #1806, #978, #3074 ) ) REPRESENTATION_CONTEXT ( 'NONE', 'WORKASPACE' ) );
#4508 = ORIENTED_EDGE ( 'NONE', *, *, #4257, .T. ) ;
#4509 = CARTESIAN_POINT ( 'NONE',  ( -213.0979982360508416, 24.99999999999997158, 511.7519955242232754 ) ) ;
#4510 = ORIENTED_EDGE ( 'NONE', *, *, #61, .F. ) ;
#4511 = CARTESIAN_POINT ( 'NONE',  ( -38.26122282208105219, -14.99999999999998579, 67.09613410133258071 ) ) ;
#4512 = AXIS2_PLACEMENT_3D ( 'NONE', #529, #3881, #604 ) ;
#4513 =( GEOMETRIC_REPRESENTATION_CONTEXT ( 3 ) GLOBAL_UNCERTAINTY_ASSIGNED_CONTEXT ( ( #3094 ) ) GLOBAL_UNIT_ASSIGNED_CONTEXT ( ( #852, #5387, #4161 ) ) REPRESENTATION_CONTEXT ( 'NONE', 'WORKASPACE' ) );
#4514 = ORIENTED_EDGE ( 'NONE', *, *, #1392, .T. ) ;
#4515 = PRODUCT_DEFINITION_CONTEXT ( 'detailed design', #4397, 'design' ) ;
#4516 = CIRCLE ( 'NONE', #3035, 50.00000000000000000 ) ;
#4517 = AXIS2_PLACEMENT_3D ( 'NONE', #5371, #698, #2412 ) ;
#4518 = AXIS2_PLACEMENT_3D ( 'NONE', #3752, #837, #5054 ) ;
#4519 = VERTEX_POINT ( 'NONE', #2122 ) ;
#4520 = PRODUCT_DEFINITION_SHAPE ( 'NONE', 'NONE',  #2322 ) ;
#4521 = CARTESIAN_POINT ( 'NONE',  ( -80.02857808274404761, 80.45434506795689344, -9.999999999999841904 ) ) ;
#4522 = CARTESIAN_POINT ( 'NONE',  ( -340.0535087002904220, -14.95948628165117178, 101.9421712359864500 ) ) ;
#4523 = PLANE ( 'NONE',  #2916 ) ;
#4524 = DIRECTION ( 'NONE',  ( 5.551115123125772841E-17, -1.848892746611743354E-31, -1.000000000000000000 ) ) ;
#4525 = AXIS2_PLACEMENT_3D ( 'NONE', #4334, #3461, #1826 ) ;
#4526 = FACE_OUTER_BOUND ( 'NONE', #2927, .T. ) ;
#4527 = AXIS2_PLACEMENT_3D ( 'NONE', #4827, #187, #4016 ) ;
#4528 = VERTEX_POINT ( 'NONE', #3726 ) ;
#4529 = FACE_OUTER_BOUND ( 'NONE', #4917, .T. ) ;
#4530 = DIRECTION ( 'NONE',  ( -0.9955873536034884896, 5.452307672560235798E-31, -0.09383933793885443353 ) ) ;
#4531 = DIRECTION ( 'NONE',  ( -0.09383933793885537722, 2.626968444144180508E-31, 0.9955873536034883786 ) ) ;
#4532 = PLANE ( 'NONE',  #3217 ) ;
#4533 = EDGE_CURVE ( 'NONE', #1814, #2651, #4247, .T. ) ;
#4534 = ADVANCED_FACE ( 'NONE', ( #5395 ), #4246, .F. ) ;
#4535 = CARTESIAN_POINT ( 'NONE',  ( -82.68018911681710392, 75.92317977368848858, -9.999999999999953815 ) ) ;
#4536 = ADVANCED_FACE ( 'NONE', ( #4577 ), #5056, .T. ) ;
#4537 = EDGE_CURVE ( 'NONE', #3805, #2756, #3290, .T. ) ;
#4538 = DIRECTION ( 'NONE',  ( -1.000000000000000000, 3.759415251443877379E-31, -5.551115123125772841E-17 ) ) ;
#4539 = CARTESIAN_POINT ( 'NONE',  ( -354.3266237013165778, 25.00000000000018474, 381.2801272015587983 ) ) ;
#4540 = CARTESIAN_POINT ( 'NONE',  ( -285.5643670724598451, 2.222614453595284090E-15, 494.2304181244439292 ) ) ;
#4541 = ORIENTED_EDGE ( 'NONE', *, *, #3331, .T. ) ;
#4542 = CARTESIAN_POINT ( 'NONE',  ( -16.96312831416352296, 1.572093150103981429E-15, 463.2830513152439380 ) ) ;
#4543 = VERTEX_POINT ( 'NONE', #2464 ) ;
#4544 = DIRECTION ( 'NONE',  ( -0.09383933793885537722, 2.626968444144180508E-31, 0.9955873536034883786 ) ) ;
#4545 = CARTESIAN_POINT ( 'NONE',  ( -349.6717162327985307, 3.252606517456513302E-16, 157.2838080833889194 ) ) ;
#4546 = ORIENTED_EDGE ( 'NONE', *, *, #1541, .T. ) ;
#4547 = AXIS2_PLACEMENT_3D ( 'NONE', #2730, #2442, #4530 ) ;
#4548 = ORIENTED_EDGE ( 'NONE', *, *, #1663, .T. ) ;
#4549 = DIRECTION ( 'NONE',  ( -0.09383933793885536334, 2.626968444144180070E-31, 0.9955873536034882676 ) ) ;
#4550 = CARTESIAN_POINT ( 'NONE',  ( 151.9714219172562650, -25.54565493204307813, -11.99999999999995559 ) ) ;
#4551 = CYLINDRICAL_SURFACE ( 'NONE', #285, 49.99999999999996447 ) ;
#4552 = ADVANCED_FACE ( 'NONE', ( #4170 ), #423, .F. ) ;
#4553 = DIRECTION ( 'NONE',  ( 1.000000000000000000, 0.000000000000000000, 0.000000000000000000 ) ) ;
#4554 = CLOSED_SHELL ( 'NONE', ( #4322, #2743, #1864, #3233, #2370, #585, #396, #3667, #4429, #3597, #1938, #4536, #5018, #2988, #3301, #4629, #2295, #2188, #2998, #4464, #1131, #3089, #3159, #258, #4187, #813, #3022, #2604, #3153, #2373, #681, #3916, #5019, #866, #2834, #2894, #230, #4293, #227, #2448, #1300, #624, #3560, #4032, #3799, #2908, #4364, #4534, #2134, #461 ) ) ;
#4555 = EDGE_CURVE ( 'NONE', #861, #3068, #385, .T. ) ;
#4556 = CARTESIAN_POINT ( 'NONE',  ( -353.4921497144319460, 2.222614453595284090E-15, 38.40071206960160310 ) ) ;
#4557 = ORIENTED_EDGE ( 'NONE', *, *, #3893, .F. ) ;
#4558 = ORIENTED_EDGE ( 'NONE', *, *, #2515, .T. ) ;
#4559 = DIRECTION ( 'NONE',  ( 0.000000000000000000, 0.000000000000000000, 1.000000000000000000 ) ) ;
#4560 = DIRECTION ( 'NONE',  ( -0.9955873536034882676, 5.484003909441380272E-31, -0.09383933793885536334 ) ) ;
#4561 = DIRECTION ( 'NONE',  ( 1.000000000000000000, 0.000000000000000000, 7.228014483236656373E-17 ) ) ;
#4562 = CARTESIAN_POINT ( 'NONE',  ( -84.02857808274407603, 84.45434506795682239, -11.99999999999995559 ) ) ;
#4563 = ADVANCED_FACE ( 'NONE', ( #5418, #3321 ), #1272, .F. ) ;
#4564 = CARTESIAN_POINT ( 'NONE',  ( -349.8593949086763928, 2.222614453595284090E-15, 159.2749827905956010 ) ) ;
#4565 = CARTESIAN_POINT ( 'NONE',  ( 4.992201166475765284, 25.00000000000018474, 252.6216919286950429 ) ) ;
#4566 = CARTESIAN_POINT ( 'NONE',  ( -105.2090356704102447, -24.99999999999981881, 560.1816718768288865 ) ) ;
#4567 = EDGE_CURVE ( 'NONE', #1142, #1648, #3467, .T. ) ;
#4568 = VERTEX_POINT ( 'NONE', #370 ) ;
#4569 = EDGE_LOOP ( 'NONE', ( #2168, #2011, #974, #3438 ) ) ;
#4570 = LINE ( 'NONE', #388, #363 ) ;
#4571 = CARTESIAN_POINT ( 'NONE',  ( -13.34676807733242754, 3.807633061153780218E-15, 36.33529372355719289 ) ) ;
#4572 = EDGE_CURVE ( 'NONE', #2971, #2111, #4506, .T. ) ;
#4573 = ORIENTED_EDGE ( 'NONE', *, *, #1301, .T. ) ;
#4574 = CARTESIAN_POINT ( 'NONE',  ( -375.4961969329172575, 3.911847525938617771E-15, 95.58821507570917220 ) ) ;
#4575 = CYLINDRICAL_SURFACE ( 'NONE', #1009, 49.99999999999996447 ) ;
#4576 = DIRECTION ( 'NONE',  ( 0.01527226085271972227, 2.095411779493299033E-31, 0.9998833722232041143 ) ) ;
#4577 = FACE_OUTER_BOUND ( 'NONE', #3673, .T. ) ;
#4578 = EDGE_LOOP ( 'NONE', ( #3212, #508 ) ) ;
#4579 = ORIENTED_EDGE ( 'NONE', *, *, #4057, .T. ) ;
#4580 = DIRECTION ( 'NONE',  ( -0.09383933793885537722, 2.626968444144180508E-31, 0.9955873536034883786 ) ) ;
#4581 = CARTESIAN_POINT ( 'NONE',  ( 137.9714219172562935, -25.54565493204318116, 152.0000000000004263 ) ) ;
#4582 = PLANE ( 'NONE',  #3478 ) ;
#4583 = ADVANCED_FACE ( 'NONE', ( #5004 ), #3797, .F. ) ;
#4584 = DIRECTION ( 'NONE',  ( -1.000000000000000000, 0.000000000000000000, -8.260587980841909197E-17 ) ) ;
#4585 = AXIS2_PLACEMENT_3D ( 'NONE', #4766, #1804, #5149 ) ;
#4586 = DIRECTION ( 'NONE',  ( -0.9955873536034882676, 5.273458392682099492E-31, -0.09383933793885600172 ) ) ;
#4587 = CARTESIAN_POINT ( 'NONE',  ( 11.65205807320727871, -24.99999999999981881, 340.0738060255407049 ) ) ;
#4588 = CARTESIAN_POINT ( 'NONE',  ( 127.9714219172562508, 80.45434506795683660, -2.000000000000002220 ) ) ;
#4589 = AXIS2_PLACEMENT_3D ( 'NONE', #4922, #1109, #1519 ) ;
#4590 = ORIENTED_EDGE ( 'NONE', *, *, #3629, .T. ) ;
#4591 = AXIS2_PLACEMENT_3D ( 'NONE', #4480, #5296, #1539 ) ;
#4592 = LINE ( 'NONE', #1625, #3670 ) ;
#4593 = AXIS2_PLACEMENT_3D ( 'NONE', #1859, #184, #269 ) ;
#4594 = EDGE_CURVE ( 'NONE', #1676, #4953, #2666, .T. ) ;
#4595 = EDGE_LOOP ( 'NONE', ( #1723, #1505, #5145, #2243 ) ) ;
#4596 = EDGE_LOOP ( 'NONE', ( #3317, #1567, #4026, #4573 ) ) ;
#4597 = ADVANCED_FACE ( 'NONE', ( #859 ), #2046, .T. ) ;
#4598 = AXIS2_PLACEMENT_3D ( 'NONE', #918, #505, #4788 ) ;
#4599 = CARTESIAN_POINT ( 'NONE',  ( -317.6377424754826393, 3.490243377570163137E-15, 121.1303224241101049 ) ) ;
#4600 = DIRECTION ( 'NONE',  ( -1.261617073437686134E-16, 1.000000000000000000, 1.232595164407830946E-31 ) ) ;
#4601 = DIRECTION ( 'NONE',  ( 5.551115123125772841E-17, -1.848892746611743135E-31, -1.000000000000000000 ) ) ;
#4602 = CARTESIAN_POINT ( 'NONE',  ( -0.8482259245422840710, 2.276824562219559311E-15, 36.14439046289818691 ) ) ;
#4603 = AXIS2_PLACEMENT_3D ( 'NONE', #4368, #595, #1453 ) ;
#4604 = AXIS2_PLACEMENT_3D ( 'NONE', #487, #4580, #809 ) ;
#4605 = ORIENTED_EDGE ( 'NONE', *, *, #4555, .F. ) ;
#4606 = ORIENTED_EDGE ( 'NONE', *, *, #3189, .T. ) ;
#4607 = CARTESIAN_POINT ( 'NONE',  ( 139.9714219172562366, -21.54565493204319182, -2.000000000000001332 ) ) ;
#4608 = AXIS2_PLACEMENT_3D ( 'NONE', #4340, #5156, #1832 ) ;
#4609 = DIRECTION ( 'NONE',  ( -0.000000000000000000, -1.000000000000000000, -0.000000000000000000 ) ) ;
#4610 = FACE_OUTER_BOUND ( 'NONE', #3961, .T. ) ;
#4611 = CIRCLE ( 'NONE', #4696, 1.000000000000000888 ) ;
#4612 = CARTESIAN_POINT ( 'NONE',  ( -213.0979982360508416, -25.00000000000003197, 511.7519955242232754 ) ) ;
#4613 = CARTESIAN_POINT ( 'NONE',  ( -336.1069982926118769, 1.517883041479706208E-15, 349.6877309229317916 ) ) ;
#4614 = CARTESIAN_POINT ( 'NONE',  ( -312.0566616799237067, 1.517883041479706208E-15, 419.2731246273846182 ) ) ;
#4615 = DIRECTION ( 'NONE',  ( -5.551115123125772841E-17, 1.848892746611743135E-31, 1.000000000000000000 ) ) ;
#4616 = MECHANICAL_DESIGN_GEOMETRIC_PRESENTATION_REPRESENTATION (  '', ( #751 ), #2163 ) ;
#4617 = VERTEX_POINT ( 'NONE', #2517 ) ;
#4618 = FACE_OUTER_BOUND ( 'NONE', #722, .T. ) ;
#4619 =( NAMED_UNIT ( * ) SI_UNIT ( $, .STERADIAN. ) SOLID_ANGLE_UNIT ( ) );
#4620 = CARTESIAN_POINT ( 'NONE',  ( 29.23877717791899400, 15.00000000000001421, 17.09613410133267664 ) ) ;
#4621 = AXIS2_PLACEMENT_3D ( 'NONE', #2456, #4159, #3234 ) ;
#4622 = ORIENTED_EDGE ( 'NONE', *, *, #869, .T. ) ;
#4623 = EDGE_CURVE ( 'NONE', #979, #664, #4193, .T. ) ;
#4624 = CARTESIAN_POINT ( 'NONE',  ( -74.02857808274399076, 80.45434506795689344, -2.000000000000112355 ) ) ;
#4625 = DIRECTION ( 'NONE',  ( -1.000000000000000000, 0.000000000000000000, 0.000000000000000000 ) ) ;
#4626 = LINE ( 'NONE', #4215, #3505 ) ;
#4627 = CARTESIAN_POINT ( 'NONE',  ( -353.5191290882918338, 0.000000000000000000, 198.1028895811327573 ) ) ;
#4628 = DIRECTION ( 'NONE',  ( -5.679099018122554920E-31, -1.000000000000000000, 2.149753974990777610E-31 ) ) ;
#4629 = ADVANCED_FACE ( 'NONE', ( #5031 ), #2541, .F. ) ;
#4630 = EDGE_CURVE ( 'NONE', #1486, #4465, #2646, .T. ) ;
#4631 = VECTOR ( 'NONE', #4772, 1000.000000000000000 ) ;
#4632 = ORIENTED_EDGE ( 'NONE', *, *, #3355, .F. ) ;
#4633 = EDGE_LOOP ( 'NONE', ( #1362, #600, #4051, #888 ) ) ;
#4634 = EDGE_LOOP ( 'NONE', ( #2839, #4234, #2324, #4268 ) ) ;
#4635 = CIRCLE ( 'NONE', #2965, 5.250000000000018652 ) ;
#4636 = CARTESIAN_POINT ( 'NONE',  ( -334.2354697480813002, -14.95948628165117178, 40.21575531256979019 ) ) ;
#4637 = CARTESIAN_POINT ( 'NONE',  ( 106.6132552010327288, 15.00000000000001421, 71.50523272244407735 ) ) ;
#4638 = DIRECTION ( 'NONE',  ( 0.000000000000000000, -1.000000000000000000, 0.000000000000000000 ) ) ;
#4639 = CARTESIAN_POINT ( 'NONE',  ( -16.96312831416352296, 1.572093150103981429E-15, 463.2830513152439380 ) ) ;
#4640 = CARTESIAN_POINT ( 'NONE',  ( -152.2642418386349163, 3.740497495074990297E-15, 532.1805559224781064 ) ) ;
#4641 = DIRECTION ( 'NONE',  ( -0.05689159511111528678, 0.000000000000000000, 0.9983803615885644689 ) ) ;
#4642 = CIRCLE ( 'NONE', #3249, 31.50000000000114397 ) ;
#4643 = EDGE_LOOP ( 'NONE', ( #3270, #1783, #3389, #2242 ) ) ;
#4644 = VERTEX_POINT ( 'NONE', #1761 ) ;
#4645 = DIRECTION ( 'NONE',  ( 1.000000000000000000, -3.759415251443877817E-31, 5.551115123125772841E-17 ) ) ;
#4646 = CARTESIAN_POINT ( 'NONE',  ( 0.000000000000000000, 0.000000000000000000, 0.000000000000000000 ) ) ;
#4647 = DIRECTION ( 'NONE',  ( -0.9955873536034882676, 5.452307672560245432E-31, -0.09383933793885568253 ) ) ;
#4648 = ORIENTED_EDGE ( 'NONE', *, *, #4594, .T. ) ;
#4649 = DIRECTION ( 'NONE',  ( -0.09383933793885568253, 2.673190762809473730E-31, 0.9955873536034882676 ) ) ;
#4650 = DIRECTION ( 'NONE',  ( 0.000000000000000000, -1.000000000000000000, 0.000000000000000000 ) ) ;
#4651 = CARTESIAN_POINT ( 'NONE',  ( -98.02857808274411866, 84.45434506795672291, 5.551115123125782702E-14 ) ) ;
#4652 = CARTESIAN_POINT ( 'NONE',  ( -357.2727026058461206, 5.421010862427522170E-17, 237.9263837252718758 ) ) ;
#4653 = CARTESIAN_POINT ( 'NONE',  ( -80.02857808274410445, -21.54565493204320248, -12.00000000000001066 ) ) ;
#4654 = EDGE_CURVE ( 'NONE', #4403, #2695, #5291, .T. ) ;
#4655 = DIRECTION ( 'NONE',  ( -5.720779902258401340E-31, -1.000000000000000000, 2.099398147291833041E-31 ) ) ;
#4656 = ORIENTED_EDGE ( 'NONE', *, *, #5089, .F. ) ;
#4657 = VERTEX_POINT ( 'NONE', #89 ) ;
#4658 = ORIENTED_EDGE ( 'NONE', *, *, #2933, .F. ) ;
#4659 = CARTESIAN_POINT ( 'NONE',  ( 128.7214219172562082, -21.54565493204319182, -2.000000000000002220 ) ) ;
#4660 = DIRECTION ( 'NONE',  ( -0.9955873536034882676, 5.498529991225541720E-31, -0.09383933793885536334 ) ) ;
#4661 = PLANE ( 'NONE',  #2321 ) ;
#4662 =( NAMED_UNIT ( * ) SI_UNIT ( $, .STERADIAN. ) SOLID_ANGLE_UNIT ( ) );
#4663 = EDGE_LOOP ( 'NONE', ( #312, #5412, #67, #2125 ) ) ;
#4664 = CARTESIAN_POINT ( 'NONE',  ( -342.0170653153606395, 3.740497495074990297E-15, 268.9367132353195302 ) ) ;
#4665 = CARTESIAN_POINT ( 'NONE',  ( -342.0170653153606395, 3.740497495074990297E-15, 268.9367132353195302 ) ) ;
#4666 = DIRECTION ( 'NONE',  ( -1.000000000000000000, 3.759415251443877379E-31, -5.551115123125772841E-17 ) ) ;
#4667 = ORIENTED_EDGE ( 'NONE', *, *, #357, .F. ) ;
#4668 = VECTOR ( 'NONE', #810, 1000.000000000000000 ) ;
#4669 = VERTEX_POINT ( 'NONE', #2212 ) ;
#4670 = DIRECTION ( 'NONE',  ( 0.09383933793885568253, -2.673190762809473730E-31, -0.9955873536034882676 ) ) ;
#4671 =( NAMED_UNIT ( * ) SI_UNIT ( $, .STERADIAN. ) SOLID_ANGLE_UNIT ( ) );
#4672 = LINE ( 'NONE', #909, #3814 ) ;
#4673 = CIRCLE ( 'NONE', #194, 12.50000000000002842 ) ;
#4674 = EDGE_LOOP ( 'NONE', ( #147, #449, #2305, #1246 ) ) ;
#4675 = DIRECTION ( 'NONE',  ( 1.000000000000000000, -3.851859888774468203E-31, 0.000000000000000000 ) ) ;
#4676 = LINE ( 'NONE', #2949, #3632 ) ;
#4677 = CARTESIAN_POINT ( 'NONE',  ( -8.629236981504860182, -25.00000000000000355, 142.6115645898824198 ) ) ;
#4678 = CIRCLE ( 'NONE', #3366, 12.50000000000009237 ) ;
#4679 = FILL_AREA_STYLE ('',( #3005 ) ) ;
#4680 = AXIS2_PLACEMENT_3D ( 'NONE', #5311, #3651, #749 ) ;
#4681 = PLANE ( 'NONE',  #1245 ) ;
#4682 = FACE_OUTER_BOUND ( 'NONE', #5345, .T. ) ;
#4683 = AXIS2_PLACEMENT_3D ( 'NONE', #893, #3864, #3518 ) ;
#4684 = ORIENTED_EDGE ( 'NONE', *, *, #2685, .F. ) ;
#4685 = ORIENTED_EDGE ( 'NONE', *, *, #2735, .T. ) ;
#4686 = PRESENTATION_LAYER_ASSIGNMENT (  '', '', ( #1613 ) ) ;
#4687 = ORIENTED_EDGE ( 'NONE', *, *, #2496, .T. ) ;
#4688 = PLANE ( 'NONE',  #805 ) ;
#4689 = DIRECTION ( 'NONE',  ( 0.09383933793885568253, -2.673190762809473730E-31, -0.9955873536034882676 ) ) ;
#4690 = VECTOR ( 'NONE', #3092, 1000.000000000000000 ) ;
#4691 = CIRCLE ( 'NONE', #2849, 5.250000000000018652 ) ;
#4692 = CARTESIAN_POINT ( 'NONE',  ( -353.5191290882918338, 0.000000000000000000, 198.1028895811323025 ) ) ;
#4693 = ORIENTED_EDGE ( 'NONE', *, *, #3746, .F. ) ;
#4694 = EDGE_CURVE ( 'NONE', #5106, #467, #2600, .T. ) ;
#4695 = CIRCLE ( 'NONE', #3995, 21.00000000000124700 ) ;
#4696 = AXIS2_PLACEMENT_3D ( 'NONE', #1247, #3806, #5422 ) ;
#4697 = DIRECTION ( 'NONE',  ( -0.9955873536034884896, 5.462637660443545995E-31, -0.09383933793885503027 ) ) ;
#4698 = ADVANCED_FACE ( 'NONE', ( #2240 ), #582, .T. ) ;
#4699 = CARTESIAN_POINT ( 'NONE',  ( -152.2642418387488874, -24.99999999999981881, 532.1805559224803801 ) ) ;
#4700 = CARTESIAN_POINT ( 'NONE',  ( -344.4167133082243595, -14.95948628165117178, 101.5309162815936048 ) ) ;
#4701 = EDGE_CURVE ( 'NONE', #864, #2228, #301, .T. ) ;
#4702 = EDGE_CURVE ( 'NONE', #4543, #2244, #1820, .T. ) ;
#4703 = EDGE_CURVE ( 'NONE', #3390, #3766, #3452, .T. ) ;
#4704 = ORIENTED_EDGE ( 'NONE', *, *, #4702, .T. ) ;
#4705 = VERTEX_POINT ( 'NONE', #3857 ) ;
#4706 = PRESENTATION_LAYER_ASSIGNMENT (  '', '', ( #751 ) ) ;
#4707 = CARTESIAN_POINT ( 'NONE',  ( -77.37696704867103392, -26.07682022631158247, -10.00000000000000888 ) ) ;
#4708 = VERTEX_POINT ( 'NONE', #4714 ) ;
#4709 = CARTESIAN_POINT ( 'NONE',  ( -1.533280346156490337, 2.222614453595284090E-15, 488.4857301958385278 ) ) ;
#4710 = VERTEX_POINT ( 'NONE', #116 ) ;
#4711 = DIRECTION ( 'NONE',  ( -1.000000000000000000, 3.759415251443877379E-31, -5.551115123125772841E-17 ) ) ;
#4712 = CARTESIAN_POINT ( 'NONE',  ( -121.8424039465433566, -24.99999999999981881, 535.4314447305355316 ) ) ;
#4713 = CARTESIAN_POINT ( 'NONE',  ( 29.77542608467492613, 2.222614453595284090E-15, 249.2409987768030533 ) ) ;
#4714 = CARTESIAN_POINT ( 'NONE',  ( 139.2214219172562650, 80.45434506795679397, -12.00000000000001066 ) ) ;
#4715 = ORIENTED_EDGE ( 'NONE', *, *, #4855, .F. ) ;
#4716 = ORIENTED_EDGE ( 'NONE', *, *, #2102, .F. ) ;
#4717 = EDGE_CURVE ( 'NONE', #1607, #2627, #2056, .T. ) ;
#4718 = VERTEX_POINT ( 'NONE', #4738 ) ;
#4719 = CARTESIAN_POINT ( 'NONE',  ( -338.5986743560152377, 14.95948628165116823, 39.80450035817695209 ) ) ;
#4720 = DIRECTION ( 'NONE',  ( 5.551115123125772841E-17, -1.848892746611743135E-31, -1.000000000000000000 ) ) ;
#4721 = CARTESIAN_POINT ( 'NONE',  ( -342.9618789639491752, 14.95948628165116823, 39.39324540378412109 ) ) ;
#4722 = PLANE ( 'NONE',  #2140 ) ;
#4723 = ORIENTED_EDGE ( 'NONE', *, *, #499, .T. ) ;
#4724 = TOROIDAL_SURFACE ( 'NONE', #2443, 30.50000000000110845, 1.000000000000000000 ) ;
#4725 = CARTESIAN_POINT ( 'NONE',  ( -323.2681027518141263, 5.712857831165387273E-15, 180.8655636403200333 ) ) ;
#4726 = CARTESIAN_POINT ( 'NONE',  ( -342.0170653153610374, -24.99999999999981881, 268.9367132353194734 ) ) ;
#4727 = DIRECTION ( 'NONE',  ( 0.9072577839912278064, -0.4205749795070158892, -5.551115123125773458E-17 ) ) ;
#4728 = ADVANCED_FACE ( 'NONE', ( #1357 ), #1969, .F. ) ;
#4729 = EDGE_CURVE ( 'NONE', #1390, #2722, #2500, .T. ) ;
#4730 = ORIENTED_EDGE ( 'NONE', *, *, #4925, .F. ) ;
#4731 = DIRECTION ( 'NONE',  ( 0.09383933793885568253, -2.673190762809473730E-31, -0.9955873536034882676 ) ) ;
#4732 = FACE_BOUND ( 'NONE', #1867, .T. ) ;
#4733 = EDGE_LOOP ( 'NONE', ( #5058, #4270, #3963, #1018 ) ) ;
#4734 = CARTESIAN_POINT ( 'NONE',  ( 11.81831109762766729, 25.00000000000000355, 46.95220429669349471 ) ) ;
#4735 = FACE_OUTER_BOUND ( 'NONE', #5083, .T. ) ;
#4736 = CARTESIAN_POINT ( 'NONE',  ( -249.5207023207451300, 1.843143693225357538E-15, 491.2832465756980014 ) ) ;
#4737 = FACE_OUTER_BOUND ( 'NONE', #4596, .T. ) ;
#4738 = CARTESIAN_POINT ( 'NONE',  ( -81.77293133282597637, -16.59391465826784540, -10.00000000000000888 ) ) ;
#4739 = EDGE_LOOP ( 'NONE', ( #3922, #5362 ) ) ;
#4740 = ORIENTED_EDGE ( 'NONE', *, *, #2457, .F. ) ;
#4741 = EDGE_LOOP ( 'NONE', ( #4248, #2542, #4864, #1431 ) ) ;
#4742 = FACE_BOUND ( 'NONE', #2508, .T. ) ;
#4743 = LINE ( 'NONE', #1881, #544 ) ;
#4744 = CARTESIAN_POINT ( 'NONE',  ( -66.30461487616335603, 15.00000000000001421, 161.8139267001887447 ) ) ;
#4745 = AXIS2_PLACEMENT_3D ( 'NONE', #2071, #2921, #5 ) ;
#4746 = EDGE_LOOP ( 'NONE', ( #3641, #3836, #4295, #5094, #4789, #3829, #4693, #4002 ) ) ;
#4747 = CARTESIAN_POINT ( 'NONE',  ( -341.0742871682481905, -6.873162489031922727E-30, 199.2758813053679887 ) ) ;
#4748 = CARTESIAN_POINT ( 'NONE',  ( -72.60637664584220374, -24.99999999999981881, 552.9197695054134556 ) ) ;
#4749 = CARTESIAN_POINT ( 'NONE',  ( -375.4961969329172575, 3.911847525938617771E-15, 95.58821507570915799 ) ) ;
#4750 = PLANE ( 'NONE',  #3762 ) ;
#4751 = CARTESIAN_POINT ( 'NONE',  ( -354.3266237013149862, 5.421010862427522170E-17, 381.2801272015580025 ) ) ;
#4752 = ORIENTED_EDGE ( 'NONE', *, *, #5189, .T. ) ;
#4753 = CARTESIAN_POINT ( 'NONE',  ( -174.3534642324304116, 5.421010862427522170E-17, 552.7876087698471110 ) ) ;
#4754 = ORIENTED_EDGE ( 'NONE', *, *, #3479, .F. ) ;
#4755 = CIRCLE ( 'NONE', #2040, 14.00000000000001243 ) ;
#4756 = CARTESIAN_POINT ( 'NONE',  ( 29.23877717791895492, -14.99999999999998579, 67.09613410133256650 ) ) ;
#4757 = CARTESIAN_POINT ( 'NONE',  ( 12.58979647763672283, 2.222614453595284090E-15, 97.46177917736021357 ) ) ;
#4758 = DIRECTION ( 'NONE',  ( -1.000000000000000000, 0.000000000000000000, 0.000000000000000000 ) ) ;
#4759 = AXIS2_PLACEMENT_3D ( 'NONE', #5030, #4601, #1271 ) ;
#4760 = ADVANCED_FACE ( 'NONE', ( #4682 ), #5191, .T. ) ;
#4761 = ADVANCED_FACE ( 'NONE', ( #2676, #4356 ), #1844, .F. ) ;
#4762 = ORIENTED_EDGE ( 'NONE', *, *, #1403, .T. ) ;
#4763 = CIRCLE ( 'NONE', #4500, 6.000000000000032863 ) ;
#4764 = EDGE_LOOP ( 'NONE', ( #3433, #550 ) ) ;
#4765 = DIRECTION ( 'NONE',  ( 0.000000000000000000, 1.000000000000000000, 0.000000000000000000 ) ) ;
#4766 = CARTESIAN_POINT ( 'NONE',  ( -353.4252897503525332, 0.000000000000000000, 197.1073022275279243 ) ) ;
#4767 = CARTESIAN_POINT ( 'NONE',  ( -357.2727026058461206, 5.421010862427522170E-17, 237.9263837252718758 ) ) ;
#4768 = CIRCLE ( 'NONE', #1785, 5.250000000000004441 ) ;
#4769 = DIRECTION ( 'NONE',  ( -0.9955873536034884896, 0.000000000000000000, -0.09383933793885443353 ) ) ;
#4770 = EDGE_LOOP ( 'NONE', ( #1986, #26, #2009, #561 ) ) ;
#4771 = AXIS2_PLACEMENT_3D ( 'NONE', #1388, #1988, #5334 ) ;
#4772 = DIRECTION ( 'NONE',  ( 0.000000000000000000, -1.000000000000000000, 0.000000000000000000 ) ) ;
#4773 = CIRCLE ( 'NONE', #476, 4.382543221487789964 ) ;
#4774 = CARTESIAN_POINT ( 'NONE',  ( -174.3534642324312358, -24.99999999999981881, 552.7876087698487027 ) ) ;
#4775 = CARTESIAN_POINT ( 'NONE',  ( -17.67824838295694434, 4.358724120770099429E-15, 47.40273599184887132 ) ) ;
#4776 = AXIS2_PLACEMENT_3D ( 'NONE', #3001, #3243, #4675 ) ;
#4777 = VECTOR ( 'NONE', #586, 1000.000000000000000 ) ;
#4778=STYLED_ITEM('',(#5451),#1285);
#4779 = ORIENTED_EDGE ( 'NONE', *, *, #3563, .T. ) ;
#4780 = EDGE_CURVE ( 'NONE', #556, #1493, #4080, .T. ) ;
#4781 = CARTESIAN_POINT ( 'NONE',  ( 35.78913469918423829, 0.000000000000000000, 310.6402212931345161 ) ) ;
#4782 = DIRECTION ( 'NONE',  ( 0.3286293958503336277, -2.131053753758135678E-19, 0.9444589563252840936 ) ) ;
#4783 = AXIS2_PLACEMENT_3D ( 'NONE', #2080, #5009, #1332 ) ;
#4784 = ORIENTED_EDGE ( 'NONE', *, *, #3783, .T. ) ;
#4785 = CARTESIAN_POINT ( 'NONE',  ( -49.96441683051492078, 25.00000000000018474, 542.4422122871054626 ) ) ;
#4786 = ORIENTED_EDGE ( 'NONE', *, *, #3974, .T. ) ;
#4787 = CARTESIAN_POINT ( 'NONE',  ( 29.23877717791899755, 0.000000000000000000, 67.09613410133263756 ) ) ;
#4788 = DIRECTION ( 'NONE',  ( 1.000000000000000000, 0.000000000000000000, 0.000000000000000000 ) ) ;
#4789 = ORIENTED_EDGE ( 'NONE', *, *, #1972, .F. ) ;
#4790 = EDGE_CURVE ( 'NONE', #907, #895, #2700, .T. ) ;
#4791 = ORIENTED_EDGE ( 'NONE', *, *, #462, .T. ) ;
#4792 = DIRECTION ( 'NONE',  ( 0.09383933793885568253, -2.673190762809473730E-31, -0.9955873536034882676 ) ) ;
#4793 = EDGE_CURVE ( 'NONE', #1648, #2973, #475, .T. ) ;
#4794 = FACE_BOUND ( 'NONE', #4764, .T. ) ;
#4795 = FACE_OUTER_BOUND ( 'NONE', #4000, .T. ) ;
#4796 = EDGE_CURVE ( 'NONE', #1151, #557, #4425, .T. ) ;
#4797 = SURFACE_STYLE_USAGE ( .BOTH. , #3131 ) ;
#4798 = ORIENTED_EDGE ( 'NONE', *, *, #1211, .T. ) ;
#4799 = FACE_OUTER_BOUND ( 'NONE', #283, .T. ) ;
#4800 = CARTESIAN_POINT ( 'NONE',  ( -223.9642223310802649, -25.00000000000003197, 534.3227077390027944 ) ) ;
#4801 = DIRECTION ( 'NONE',  ( -0.000000000000000000, -1.000000000000000000, -0.000000000000000000 ) ) ;
#4802 = CARTESIAN_POINT ( 'NONE',  ( 11.65031622824785984, 2.276824562219551028E-15, 35.95348720223918804 ) ) ;
#4803 = ORIENTED_EDGE ( 'NONE', *, *, #2679, .F. ) ;
#4804 = FACE_OUTER_BOUND ( 'NONE', #1217, .T. ) ;
#4805 = ORIENTED_EDGE ( 'NONE', *, *, #5257, .F. ) ;
#4806 = CARTESIAN_POINT ( 'NONE',  ( 12.58979647763662513, 25.00000000000000355, 97.46177917735926144 ) ) ;
#4807 = EDGE_LOOP ( 'NONE', ( #52, #2284, #806 ) ) ;
#4808 = DIRECTION ( 'NONE',  ( -5.551115123125772841E-17, 1.848892746611743135E-31, 1.000000000000000000 ) ) ;
#4809 = SURFACE_SIDE_STYLE ('',( #3999 ) ) ;
#4810 = ORIENTED_EDGE ( 'NONE', *, *, #4572, .F. ) ;
#4811 = ORIENTED_EDGE ( 'NONE', *, *, #4363, .F. ) ;
#4812 = EDGE_CURVE ( 'NONE', #3719, #697, #4434, .T. ) ;
#4813 = FACE_OUTER_BOUND ( 'NONE', #3149, .T. ) ;
#4814 = PLANE ( 'NONE',  #4373 ) ;
#4815 = CARTESIAN_POINT ( 'NONE',  ( -338.5986743560152377, -14.95948628165117178, 39.80450035817695209 ) ) ;
#4816 = FACE_OUTER_BOUND ( 'NONE', #40, .T. ) ;
#4817 = DIRECTION ( 'NONE',  ( 0.9955873536034884896, -5.462637660443545995E-31, 0.09383933793885503027 ) ) ;
#4818 = ORIENTED_EDGE ( 'NONE', *, *, #1264, .T. ) ;
#4819 = DIRECTION ( 'NONE',  ( 5.551115123125772841E-17, -1.848892746611743135E-31, -1.000000000000000000 ) ) ;
#4820 = CARTESIAN_POINT ( 'NONE',  ( 139.9714219172562650, -21.54565493204319182, -12.00000000000006573 ) ) ;
#4821 = CARTESIAN_POINT ( 'NONE',  ( -19.78983854945535725, -24.99999999999981881, 515.1268587725797943 ) ) ;
#4822 = DIRECTION ( 'NONE',  ( 1.000000000000000000, 0.000000000000000000, 8.260587980841909197E-17 ) ) ;
#4823 = EDGE_CURVE ( 'NONE', #4034, #4718, #5386, .T. ) ;
#4824 = DIRECTION ( 'NONE',  ( 0.01527226085271972227, 2.095411779493299033E-31, 0.9998833722232041143 ) ) ;
#4825 = ORIENTED_EDGE ( 'NONE', *, *, #4151, .T. ) ;
#4826 = CARTESIAN_POINT ( 'NONE',  ( -19.78983854945535725, 25.00000000000018474, 515.1268587725797943 ) ) ;
#4827 = CARTESIAN_POINT ( 'NONE',  ( 0.000000000000000000, 0.000000000000000000, 0.000000000000000000 ) ) ;
#4828 = CARTESIAN_POINT ( 'NONE',  ( 35.78913469918393275, -24.99999999999981881, 310.6402212931347435 ) ) ;
#4829 = EDGE_LOOP ( 'NONE', ( #2983, #38 ) ) ;
#4830 = CARTESIAN_POINT ( 'NONE',  ( -152.2642418385221674, 25.00000000000018474, 532.1805559224801527 ) ) ;
#4831 = VERTEX_POINT ( 'NONE', #280 ) ;
#4832 = DIRECTION ( 'NONE',  ( 0.4205749795070160557, -0.9072577839912276954, -5.551115123125780853E-17 ) ) ;
#4833 = DIRECTION ( 'NONE',  ( -5.551115123125785167E-17, 0.000000000000000000, -1.000000000000000000 ) ) ;
#4834 = ORIENTED_EDGE ( 'NONE', *, *, #4701, .F. ) ;
#4835 = ORIENTED_EDGE ( 'NONE', *, *, #3318, .F. ) ;
#4836 = DIRECTION ( 'NONE',  ( 0.000000000000000000, -1.000000000000000000, 0.000000000000000000 ) ) ;
#4837 = CIRCLE ( 'NONE', #3280, 1.000000000000000888 ) ;
#4838 = FACE_OUTER_BOUND ( 'NONE', #172, .T. ) ;
#4839 = CARTESIAN_POINT ( 'NONE',  ( -332.6117946626184221, -1.154691298157368797E-29, 200.0735156778482917 ) ) ;
#4840 = PLANE ( 'NONE',  #1450 ) ;
#4841 = DIRECTION ( 'NONE',  ( -5.551115123125772841E-17, 1.848892746611743135E-31, 1.000000000000000000 ) ) ;
#4842 = ORIENTED_EDGE ( 'NONE', *, *, #1046, .T. ) ;
#4843 = CIRCLE ( 'NONE', #4759, 5.250000000000018652 ) ;
#4844 =( NAMED_UNIT ( * ) PLANE_ANGLE_UNIT ( ) SI_UNIT ( $, .RADIAN. ) );
#4845 = APPLICATION_CONTEXT ( 'automotive_design' ) ;
#4846 = CARTESIAN_POINT ( 'NONE',  ( -80.02857808274418971, -21.54565493204321669, -2.000000000000001776 ) ) ;
#4847 = CARTESIAN_POINT ( 'NONE',  ( 127.9714219172562224, 80.45434506795683660, -12.00000000000001066 ) ) ;
#4848 = CARTESIAN_POINT ( 'NONE',  ( -80.02857808274401918, 80.45434506795689344, -2.000000000000112799 ) ) ;
#4849 = CIRCLE ( 'NONE', #4591, 14.00000000000001243 ) ;
#4850 = AXIS2_PLACEMENT_3D ( 'NONE', #5339, #3238, #716 ) ;
#4851 = LINE ( 'NONE', #1091, #4416 ) ;
#4852 = VECTOR ( 'NONE', #1028, 1000.000000000000000 ) ;
#4853 = EDGE_CURVE ( 'NONE', #2244, #1807, #4916, .T. ) ;
#4854 = VECTOR ( 'NONE', #4007, 1000.000000000000000 ) ;
#4855 = EDGE_CURVE ( 'NONE', #4277, #860, #1130, .T. ) ;
#4856 = DIRECTION ( 'NONE',  ( 5.551115123125772841E-17, -1.848892746611743135E-31, -1.000000000000000000 ) ) ;
#4857 = CARTESIAN_POINT ( 'NONE',  ( -80.60298687151650654, 2.222614453595284090E-15, 555.2885198911399129 ) ) ;
#4858 = CARTESIAN_POINT ( 'NONE',  ( -80.59222536594943165, -24.99999999999981881, 529.1597157429057461 ) ) ;
#4859 = CARTESIAN_POINT ( 'NONE',  ( 36.35777514575885760, 2.222614453595284090E-15, 354.7349908125909792 ) ) ;
#4860 = EDGE_CURVE ( 'NONE', #4985, #1728, #4255, .T. ) ;
#4861 = VECTOR ( 'NONE', #2283, 1000.000000000000000 ) ;
#4862 = EDGE_CURVE ( 'NONE', #5281, #5060, #1875, .T. ) ;
#4863 = VECTOR ( 'NONE', #4615, 1000.000000000000000 ) ;
#4864 = ORIENTED_EDGE ( 'NONE', *, *, #4533, .T. ) ;
#4865 = CARTESIAN_POINT ( 'NONE',  ( -107.0991749147297014, 25.00000000000018474, 535.0680222229608489 ) ) ;
#4866 = ORIENTED_EDGE ( 'NONE', *, *, #3721, .F. ) ;
#4867 = VECTOR ( 'NONE', #3305, 1000.000000000000000 ) ;
#4868 = DIRECTION ( 'NONE',  ( -0.09383933793885536334, 2.626968444144180070E-31, 0.9955873536034882676 ) ) ;
#4869 = AXIS2_PLACEMENT_3D ( 'NONE', #374, #4176, #5007 ) ;
#4870 = CARTESIAN_POINT ( 'NONE',  ( -77.37696704867106234, 84.98551036222526989, -9.999999999999953815 ) ) ;
#4871 = VERTEX_POINT ( 'NONE', #4870 ) ;
#4872 = EDGE_LOOP ( 'NONE', ( #4044, #500, #2280, #474, #1823, #590, #2380 ) ) ;
#4873 = CARTESIAN_POINT ( 'NONE',  ( -344.4167133082243595, 2.222614453595284090E-15, 101.5309162815936048 ) ) ;
#4874 = CARTESIAN_POINT ( 'NONE',  ( -347.9826081498995336, 2.222614453595284090E-15, 139.3632357185260560 ) ) ;
#4875 = CARTESIAN_POINT ( 'NONE',  ( -60.76122282208098824, -14.99999999999998579, 167.0961341013325523 ) ) ;
#4876 = DIRECTION ( 'NONE',  ( -5.551115123125772841E-17, 1.848892746611743135E-31, 1.000000000000000000 ) ) ;
#4877 = ORIENTED_EDGE ( 'NONE', *, *, #2647, .F. ) ;
#4878 = EDGE_CURVE ( 'NONE', #689, #3599, #2369, .T. ) ;
#4879 = PLANE ( 'NONE',  #2667 ) ;
#4880 = CARTESIAN_POINT ( 'NONE',  ( -223.9642223310785312, 5.421010862427522170E-17, 534.3227077389987016 ) ) ;
#4881 = CARTESIAN_POINT ( 'NONE',  ( -84.02857808274418971, -25.54565493204318116, -5.551115123125782702E-14 ) ) ;
#4882 = DIRECTION ( 'NONE',  ( -0.4205749795070160557, 0.9072577839912276954, 5.551115123125780853E-17 ) ) ;
#4883 = CYLINDRICAL_SURFACE ( 'NONE', #2187, 4.382543221487789964 ) ;
#4884 = CARTESIAN_POINT ( 'NONE',  ( -249.5207023207449879, 24.99999999999997158, 491.2832465756976035 ) ) ;
#4885 = EDGE_CURVE ( 'NONE', #606, #2924, #3614, .T. ) ;
#4886 = CARTESIAN_POINT ( 'NONE',  ( 23.50217280488020677, 5.421010862427522170E-17, 428.9062724124374881 ) ) ;
#4887 = LINE ( 'NONE', #1124, #2226 ) ;
#4888 = ORIENTED_EDGE ( 'NONE', *, *, #1972, .T. ) ;
#4889 = CARTESIAN_POINT ( 'NONE',  ( -342.0244061588616091, 25.00000000000018474, 297.0039604601892620 ) ) ;
#4890 = ORIENTED_EDGE ( 'NONE', *, *, #4230, .T. ) ;
#4891 = CIRCLE ( 'NONE', #2529, 30.50000000000124345 ) ;
#4892 = FACE_OUTER_BOUND ( 'NONE', #3422, .T. ) ;
#4893 = SURFACE_STYLE_USAGE ( .BOTH. , #4809 ) ;
#4894 = ORIENTED_EDGE ( 'NONE', *, *, #1036, .F. ) ;
#4895 = UNCERTAINTY_MEASURE_WITH_UNIT (LENGTH_MEASURE( 1.000000000000000082E-05 ), #1289, 'distance_accuracy_value', 'NONE');
#4896 = ORIENTED_EDGE ( 'NONE', *, *, #1284, .F. ) ;
#4897 = DIRECTION ( 'NONE',  ( -1.000000000000000000, 0.000000000000000000, 0.000000000000000000 ) ) ;
#4898 = DIRECTION ( 'NONE',  ( 0.9955873536034882676, -5.273458392682099492E-31, 0.09383933793885600172 ) ) ;
#4899 = CARTESIAN_POINT ( 'NONE',  ( 133.9714219172562366, -21.54565493204319182, -26.84924240491753977 ) ) ;
#4900 = DIRECTION ( 'NONE',  ( -0.9955873536034882676, 5.436595176548168253E-31, -0.09383933793885512742 ) ) ;
#4901 = ORIENTED_EDGE ( 'NONE', *, *, #2982, .F. ) ;
#4902 = CARTESIAN_POINT ( 'NONE',  ( 136.6230329513292645, -17.01448963777482248, -12.00000000000001066 ) ) ;
#4903 = DIRECTION ( 'NONE',  ( -0.9072577839912275843, -0.4205749795070160002, -1.110223024625155801E-16 ) ) ;
#4904 = FACE_OUTER_BOUND ( 'NONE', #2918, .T. ) ;
#4905 = CARTESIAN_POINT ( 'NONE',  ( 96.73877717791896202, 0.000000000000000000, 67.09613410133256650 ) ) ;
#4906 = PRODUCT_DEFINITION_SHAPE ( 'NONE', 'NONE',  #5436 ) ;
#4907 = CYLINDRICAL_SURFACE ( 'NONE', #1252, 14.00000000000002665 ) ;
#4908 = DIRECTION ( 'NONE',  ( -0.09383933793885537722, 2.626968444144180508E-31, 0.9955873536034883786 ) ) ;
#4909 = CARTESIAN_POINT ( 'NONE',  ( -312.0566616799260373, 24.99999999999997158, 419.2731246273838792 ) ) ;
#4910 = CARTESIAN_POINT ( 'NONE',  ( 11.81831109762787690, 2.222614453595284090E-15, 46.95220429669389262 ) ) ;
#4911 = ORIENTED_EDGE ( 'NONE', *, *, #2524, .T. ) ;
#4912 = CARTESIAN_POINT ( 'NONE',  ( -264.1404626571541598, 24.99999999999997158, 511.7445549721641100 ) ) ;
#4913 = CIRCLE ( 'NONE', #4483, 1.000000000000000888 ) ;
#4914 = ORIENTED_EDGE ( 'NONE', *, *, #1664, .T. ) ;
#4915 = CARTESIAN_POINT ( 'NONE',  ( -378.9271552156734515, 5.590393151250690779E-15, 174.6149733621406028 ) ) ;
#4916 = LINE ( 'NONE', #2397, #3903 ) ;
#4917 = EDGE_LOOP ( 'NONE', ( #1186, #4685, #3172, #2098 ) ) ;
#4918 = VERTEX_POINT ( 'NONE', #314 ) ;
#4919 = FACE_OUTER_BOUND ( 'NONE', #425, .T. ) ;
#4920 = FACE_OUTER_BOUND ( 'NONE', #3573, .T. ) ;
#4921 = EDGE_CURVE ( 'NONE', #4871, #4528, #710, .T. ) ;
#4922 = CARTESIAN_POINT ( 'NONE',  ( -353.5191290882918338, 0.000000000000000000, 198.1028895811323025 ) ) ;
#4923 = DIRECTION ( 'NONE',  ( -0.9955873536034882676, 5.498835694391114214E-31, -0.09383933793885514130 ) ) ;
#4924 = EDGE_CURVE ( 'NONE', #4718, #1930, #3644, .T. ) ;
#4925 = EDGE_CURVE ( 'NONE', #1574, #2554, #646, .T. ) ;
#4927 = MANIFOLD_SOLID_BREP ( 'Sweep1', #4461 ) ;
#4926 = DIRECTION ( 'NONE',  ( 0.09383933793885568253, -2.673190762809473730E-31, -0.9955873536034882676 ) ) ;
#4928 = ORIENTED_EDGE ( 'NONE', *, *, #4363, .T. ) ;
#4929 = CIRCLE ( 'NONE', #3877, 5.250000000000004441 ) ;
#4930 =( LENGTH_UNIT ( ) NAMED_UNIT ( * ) SI_UNIT ( .MILLI., .METRE. ) );
#4931 = CARTESIAN_POINT ( 'NONE',  ( -353.4921497144319460, 2.222614453595284090E-15, 38.40071206960160310 ) ) ;
#4932 = CARTESIAN_POINT ( 'NONE',  ( -360.7307227603793649, 2.222614453595284090E-15, 354.4373729494858480 ) ) ;
#4933 = DIRECTION ( 'NONE',  ( 5.551115123125772841E-17, -1.848892746611743354E-31, -1.000000000000000000 ) ) ;
#4934 = CIRCLE ( 'NONE', #2833, 23.00000000000121503 ) ;
#4935 =( NAMED_UNIT ( * ) PLANE_ANGLE_UNIT ( ) SI_UNIT ( $, .RADIAN. ) );
#4936 = AXIS2_PLACEMENT_3D ( 'NONE', #629, #2309, #3996 ) ;
#4937 = CARTESIAN_POINT ( 'NONE',  ( 133.9714219172562650, 80.45434506795683660, -2.000000000000001776 ) ) ;
#4938 = AXIS2_PLACEMENT_3D ( 'NONE', #4873, #199, #2843 ) ;
#4939 = CARTESIAN_POINT ( 'NONE',  ( -367.0460729392618191, 25.00000000000018474, 268.0688838304706678 ) ) ;
#4940 = CONTEXT_DEPENDENT_SHAPE_REPRESENTATION ( #2325, #2507 ) ;
#4941 = CARTESIAN_POINT ( 'NONE',  ( -207.8397519515728504, 5.421010862427522170E-17, 541.5412455041541762 ) ) ;
#4942 = ADVANCED_FACE ( 'NONE', ( #1901, #746 ), #3174, .F. ) ;
#4943 = AXIS2_PLACEMENT_3D ( 'NONE', #609, #1397, #5199 ) ;
#4944 = AXIS2_PLACEMENT_3D ( 'NONE', #1448, #3099, #4769 ) ;
#4945 = ORIENTED_EDGE ( 'NONE', *, *, #2999, .T. ) ;
#4946 = CARTESIAN_POINT ( 'NONE',  ( 11.35554381052501682, 25.00000000000018474, 353.5846600851141943 ) ) ;
#4947 = EDGE_LOOP ( 'NONE', ( #4684, #2178 ) ) ;
#4948 = ADVANCED_FACE ( 'NONE', ( #3235 ), #2752, .F. ) ;
#4949 = CARTESIAN_POINT ( 'NONE',  ( -351.7361816674535362, 5.421010862427522170E-17, 179.1867298626658283 ) ) ;
#4950 = AXIS2_PLACEMENT_3D ( 'NONE', #4602, #2489, #1652 ) ;
#4951 = AXIS2_PLACEMENT_3D ( 'NONE', #1970, #1141, #4494 ) ;
#4952 = FACE_OUTER_BOUND ( 'NONE', #3000, .T. ) ;
#4953 = VERTEX_POINT ( 'NONE', #364 ) ;
#4954 = AXIS2_PLACEMENT_3D ( 'NONE', #3603, #268, #4100 ) ;
#4955 = AXIS2_PLACEMENT_3D ( 'NONE', #2129, #1712, #5062 ) ;
#4956 = ORIENTED_EDGE ( 'NONE', *, *, #2982, .T. ) ;
#4957 = CARTESIAN_POINT ( 'NONE',  ( -98.02857808274420393, -25.54565493204309234, 5.551115123125782702E-14 ) ) ;
#4958 = DIRECTION ( 'NONE',  ( 0.09383933793885537722, -2.626968444144180508E-31, -0.9955873536034883786 ) ) ;
#4959 = DIRECTION ( 'NONE',  ( -1.219242865862094703E-16, 1.000000000000000000, -1.149200448409285278E-17 ) ) ;
#4960 = PLANE ( 'NONE',  #2138 ) ;
#4961 = AXIS2_PLACEMENT_3D ( 'NONE', #2247, #3154, #2684 ) ;
#4962 = ADVANCED_FACE ( 'NONE', ( #1594 ), #1352, .T. ) ;
#4963 = CARTESIAN_POINT ( 'NONE',  ( -84.02857808274397655, 98.45434506795682239, 152.0000000000000853 ) ) ;
#4964 = ORIENTED_EDGE ( 'NONE', *, *, #490, .F. ) ;
#4965 = ORIENTED_EDGE ( 'NONE', *, *, #2078, .F. ) ;
#4966 = CARTESIAN_POINT ( 'NONE',  ( -378.1800370315194186, 2.571758278209485443E-15, 235.9557576285559151 ) ) ;
#4967 = ADVANCED_FACE ( 'NONE', ( #1645 ), #3788, .T. ) ;
#4968 = CARTESIAN_POINT ( 'NONE',  ( -84.02857808274397655, 98.45434506795682239, 152.0000000000000853 ) ) ;
#4969 = CYLINDRICAL_SURFACE ( 'NONE', #3024, 6.000000000000032863 ) ;
#4970 = PLANE ( 'NONE',  #2357 ) ;
#4971 = CARTESIAN_POINT ( 'NONE',  ( 8.821273309659243722, 25.00000000000018474, 380.5076279642384520 ) ) ;
#4972 = CARTESIAN_POINT ( 'NONE',  ( -223.9642223310802649, -25.00000000000003197, 534.3227077390027944 ) ) ;
#4973 = ORIENTED_EDGE ( 'NONE', *, *, #1535, .F. ) ;
#4974 = ORIENTED_EDGE ( 'NONE', *, *, #617, .F. ) ;
#4975 = CARTESIAN_POINT ( 'NONE',  ( -84.02857808274413287, 84.45434506795682239, -5.551115123125782702E-14 ) ) ;
#4976 = CARTESIAN_POINT ( 'NONE',  ( -353.5191290882918338, 0.000000000000000000, 198.1028895811327573 ) ) ;
#4977 = MANIFOLD_SOLID_BREP ( 'Boss-Extrude1', #3147 ) ;
#4978 = ORIENTED_EDGE ( 'NONE', *, *, #4703, .F. ) ;
#4979 = CARTESIAN_POINT ( 'NONE',  ( -108.3530091724271358, 15.00000000000001421, 123.8676211295743599 ) ) ;
#4980 = LINE ( 'NONE', #5029, #2553 ) ;
#4981 = DIRECTION ( 'NONE',  ( -1.000000000000000000, 0.000000000000000000, 0.000000000000000000 ) ) ;
#4982 = DIRECTION ( 'NONE',  ( -1.219242865862094703E-16, 1.000000000000000000, -1.149200448409289593E-17 ) ) ;
#4983 = CIRCLE ( 'NONE', #3242, 28.50000000000127898 ) ;
#4984 = ORIENTED_EDGE ( 'NONE', *, *, #5228, .T. ) ;
#4985 = VERTEX_POINT ( 'NONE', #4571 ) ;
#4986 = CARTESIAN_POINT ( 'NONE',  ( -80.02857808274401918, 80.45434506795689344, -2.000000000000112799 ) ) ;
#4987 = DIRECTION ( 'NONE',  ( 5.551115123125772841E-17, -1.848892746611743354E-31, -1.000000000000000000 ) ) ;
#4988 = DIRECTION ( 'NONE',  ( -0.9955873536034882676, 5.452307672560250687E-31, -0.09383933793885569641 ) ) ;
#4989 = CARTESIAN_POINT ( 'NONE',  ( -321.8445680969931004, 4.999156891862629509E-15, 103.6584595401686357 ) ) ;
#4990 = CARTESIAN_POINT ( 'NONE',  ( -12.39202333278749357, 1.572093150103981429E-15, 98.84296066633379496 ) ) ;
#4991 = CARTESIAN_POINT ( 'NONE',  ( -8.629236981521737349, 1.572093150103981429E-15, 142.6115645898827893 ) ) ;
#4992 = DIRECTION ( 'NONE',  ( -0.9955873536034882676, 5.453577263127812432E-31, -0.09383933793885552987 ) ) ;
#4993 = EDGE_CURVE ( 'NONE', #1199, #2087, #1261, .T. ) ;
#4994 = EDGE_CURVE ( 'NONE', #3556, #5300, #5049, .T. ) ;
#4995 = VERTEX_POINT ( 'NONE', #1291 ) ;
#4996 = CARTESIAN_POINT ( 'NONE',  ( -353.5191290882918338, 0.000000000000000000, 198.1028895811323025 ) ) ;
#4997 = CARTESIAN_POINT ( 'NONE',  ( -353.5191290882918338, 0.000000000000000000, 198.1028895811327573 ) ) ;
#4998 = ORIENTED_EDGE ( 'NONE', *, *, #1228, .T. ) ;
#4999 = EDGE_LOOP ( 'NONE', ( #2710, #3646, #3801, #5220 ) ) ;
#5000 = PRODUCT_RELATED_PRODUCT_CATEGORY ( 'part', '', ( #835 ) ) ;
#5001 = FACE_OUTER_BOUND ( 'NONE', #3775, .T. ) ;
#5002 = DIRECTION ( 'NONE',  ( -0.9955873536034882676, 5.452980219524763634E-31, -0.09383933793885573804 ) ) ;
#5003 = DIRECTION ( 'NONE',  ( -0.9955873536034886007, 6.162975822039140717E-31, -0.09383933793885225472 ) ) ;
#5004 = FACE_OUTER_BOUND ( 'NONE', #973, .T. ) ;
#5005 = ORIENTED_EDGE ( 'NONE', *, *, #2078, .T. ) ;
#5006 = VERTEX_POINT ( 'NONE', #4136 ) ;
#5007 = DIRECTION ( 'NONE',  ( -0.9955873536034882676, 5.452980219524763634E-31, -0.09383933793885573804 ) ) ;
#5008 = DIRECTION ( 'NONE',  ( -1.000000000000000000, 3.759415251443877379E-31, -5.551115123125772841E-17 ) ) ;
#5009 = DIRECTION ( 'NONE',  ( 0.09383933793885537722, -2.626968444144180508E-31, -0.9955873536034883786 ) ) ;
#5010 = AXIS2_PLACEMENT_3D ( 'NONE', #2287, #4720, #1469 ) ;
#5011 = CARTESIAN_POINT ( 'NONE',  ( -152.2642418386349163, 3.740497495074990297E-15, 532.1805559224781064 ) ) ;
#5012 = CARTESIAN_POINT ( 'NONE',  ( 11.65205807320734976, 3.740497495074990297E-15, 340.0738060255405912 ) ) ;
#5013 = CARTESIAN_POINT ( 'NONE',  ( 137.9714219172563219, 84.45434506795683660, 152.0000000000003126 ) ) ;
#5014 = AXIS2_PLACEMENT_3D ( 'NONE', #2319, #668, #4898 ) ;
#5015 = EDGE_CURVE ( 'NONE', #1449, #5006, #2671, .T. ) ;
#5016 = ORIENTED_EDGE ( 'NONE', *, *, #1325, .F. ) ;
#5017 = CIRCLE ( 'NONE', #1249, 49.99999999999996447 ) ;
#5018 = ADVANCED_FACE ( 'NONE', ( #4952 ), #1626, .T. ) ;
#5019 = ADVANCED_FACE ( 'NONE', ( #2510 ), #878, .T. ) ;
#5020 = DIRECTION ( 'NONE',  ( -5.679099018122554920E-31, -1.000000000000000000, 2.149753974990777610E-31 ) ) ;
#5021 = EDGE_CURVE ( 'NONE', #861, #4306, #35, .T. ) ;
#5022 = DIRECTION ( 'NONE',  ( -3.204747427460360459E-31, 1.000000000000000000, -1.848892746611743354E-31 ) ) ;
#5023 = CIRCLE ( 'NONE', #5288, 5.250000000000018652 ) ;
#5024 = VERTEX_POINT ( 'NONE', #3748 ) ;
#5025 = AXIS2_PLACEMENT_3D ( 'NONE', #3588, #5246, #2721 ) ;
#5026 = CIRCLE ( 'NONE', #302, 4.382543221487789076 ) ;
#5027 = DIRECTION ( 'NONE',  ( -0.09383933793885568253, 2.673190762809473730E-31, 0.9955873536034882676 ) ) ;
#5028 = CARTESIAN_POINT ( 'NONE',  ( -357.8553543223658835, 2.759321206427282701E-15, 37.98945711520877211 ) ) ;
#5029 = CARTESIAN_POINT ( 'NONE',  ( -98.02857808274411866, 84.45434506795672291, -12.00000000000001066 ) ) ;
#5030 = CARTESIAN_POINT ( 'NONE',  ( -80.02857808274410445, -21.54565493204320248, -12.00000000000001066 ) ) ;
#5031 = FACE_OUTER_BOUND ( 'NONE', #447, .T. ) ;
#5032 = AXIS2_PLACEMENT_3D ( 'NONE', #1965, #2346, #1575 ) ;
#5033 = AXIS2_PLACEMENT_3D ( 'NONE', #77, #2993, #4666 ) ;
#5034 = CIRCLE ( 'NONE', #4869, 31.50000000000120082 ) ;
#5035 = ORIENTED_EDGE ( 'NONE', *, *, #1853, .T. ) ;
#5036 = ORIENTED_EDGE ( 'NONE', *, *, #3394, .F. ) ;
#5037 = VERTEX_POINT ( 'NONE', #416 ) ;
#5038 = FACE_OUTER_BOUND ( 'NONE', #5310, .T. ) ;
#5039 = CIRCLE ( 'NONE', #1359, 1.000000000000000888 ) ;
#5040 = LINE ( 'NONE', #2546, #4668 ) ;
#5041 = CARTESIAN_POINT ( 'NONE',  ( -373.4844736152189171, 3.367778697655401957E-15, 116.8709068531373703 ) ) ;
#5042 = CARTESIAN_POINT ( 'NONE',  ( 6.585909452853061730, 3.740497495074990297E-15, 393.9228865916071527 ) ) ;
#5043 = CARTESIAN_POINT ( 'NONE',  ( -336.1069982926118769, 1.517883041479706208E-15, 349.6877309229317916 ) ) ;
#5044 = DIRECTION ( 'NONE',  ( 1.000000000000000000, 0.000000000000000000, 0.000000000000000000 ) ) ;
#5045 = ORIENTED_EDGE ( 'NONE', *, *, #1083, .F. ) ;
#5046 = EDGE_CURVE ( 'NONE', #5400, #1486, #739, .T. ) ;
#5047 = EDGE_LOOP ( 'NONE', ( #962, #569, #2453, #4752 ) ) ;
#5048 = CARTESIAN_POINT ( 'NONE',  ( -330.7350079038403123, 5.421010862426367228E-17, 180.1617686057784056 ) ) ;
#5049 = LINE ( 'NONE', #4620, #1006 ) ;
#5050 = VERTEX_POINT ( 'NONE', #1 ) ;
#5051 = LINE ( 'NONE', #721, #3648 ) ;
#5052 = CARTESIAN_POINT ( 'NONE',  ( -338.5986743560152377, -14.95948628165117178, 39.80450035817695209 ) ) ;
#5053 = CYLINDRICAL_SURFACE ( 'NONE', #3980, 56.63911695420845405 ) ;
#5054 = DIRECTION ( 'NONE',  ( 0.000000000000000000, 0.000000000000000000, 1.000000000000000000 ) ) ;
#5055 = FACE_OUTER_BOUND ( 'NONE', #5118, .T. ) ;
#5056 = PLANE ( 'NONE',  #1873 ) ;
#5057 = VECTOR ( 'NONE', #571, 1000.000000000000000 ) ;
#5058 = ORIENTED_EDGE ( 'NONE', *, *, #1635, .F. ) ;
#5059 = ORIENTED_EDGE ( 'NONE', *, *, #1664, .F. ) ;
#5060 = VERTEX_POINT ( 'NONE', #3362 ) ;
#5061 = VECTOR ( 'NONE', #3569, 1000.000000000000000 ) ;
#5062 = DIRECTION ( 'NONE',  ( -0.9955873536034881566, 5.462637660443544243E-31, -0.09383933793885600172 ) ) ;
#5063 = AXIS2_PLACEMENT_3D ( 'NONE', #3934, #986, #619 ) ;
#5064 = CARTESIAN_POINT ( 'NONE',  ( -84.02857808274407603, 84.45434506795682239, -11.99999999999995559 ) ) ;
#5065 = DIRECTION ( 'NONE',  ( -5.551115123125772841E-17, 1.848892746611743135E-31, 1.000000000000000000 ) ) ;
#5066 = CARTESIAN_POINT ( 'NONE',  ( 133.9714219172562366, -21.54565493204319182, -2.000000000000001776 ) ) ;
#5067 = ORIENTED_EDGE ( 'NONE', *, *, #1060, .F. ) ;
#5068 = EDGE_CURVE ( 'NONE', #5098, #3703, #2997, .T. ) ;
#5069 = DIRECTION ( 'NONE',  ( 0.000000000000000000, 1.000000000000000000, 0.000000000000000000 ) ) ;
#5070 = CARTESIAN_POINT ( 'NONE',  ( -63.04765821499436385, 1.843143693225357538E-15, 521.0401840782876661 ) ) ;
#5071 = ORIENTED_EDGE ( 'NONE', *, *, #4304, .F. ) ;
#5072 = ORIENTED_EDGE ( 'NONE', *, *, #3328, .F. ) ;
#5073 = LINE ( 'NONE', #53, #1757 ) ;
#5074 = DIRECTION ( 'NONE',  ( -0.05689159511111523820, 0.000000000000000000, 0.9983803615885644689 ) ) ;
#5075 = ORIENTED_EDGE ( 'NONE', *, *, #4796, .T. ) ;
#5076 = CARTESIAN_POINT ( 'NONE',  ( -38.26122282208105219, -14.99999999999998579, 67.09613410133258071 ) ) ;
#5077 = CARTESIAN_POINT ( 'NONE',  ( -338.5986743560152377, 14.95948628165116823, 39.80450035817695209 ) ) ;
#5078 = CARTESIAN_POINT ( 'NONE',  ( -107.0991749147297014, -24.99999999999981881, 535.0680222229608489 ) ) ;
#5079 =( LENGTH_UNIT ( ) NAMED_UNIT ( * ) SI_UNIT ( .MILLI., .METRE. ) );
#5080 = CARTESIAN_POINT ( 'NONE',  ( 133.9714219172562366, -21.54565493204319182, -2.000000000000001776 ) ) ;
#5081 = CARTESIAN_POINT ( 'NONE',  ( -0.6802310551622114954, 2.222614453595284090E-15, 47.14310755735262859 ) ) ;
#5082 = VECTOR ( 'NONE', #3361, 1000.000000000000114 ) ;
#5083 = EDGE_LOOP ( 'NONE', ( #4805, #890, #519, #2791 ) ) ;
#5084 = ORIENTED_EDGE ( 'NONE', *, *, #5283, .T. ) ;
#5085 = EDGE_CURVE ( 'NONE', #1327, #4236, #4672, .T. ) ;
#5086 = ADVANCED_FACE ( 'NONE', ( #55, #2591 ), #1727, .T. ) ;
#5087 = ORIENTED_EDGE ( 'NONE', *, *, #4853, .F. ) ;
#5088 = FACE_BOUND ( 'NONE', #2399, .T. ) ;
#5089 = EDGE_CURVE ( 'NONE', #3674, #4331, #2375, .T. ) ;
#5090 = DIRECTION ( 'NONE',  ( -5.551115123125772841E-17, 1.848892746611743135E-31, 1.000000000000000000 ) ) ;
#5091 = PLANE ( 'NONE',  #4783 ) ;
#5092 = ADVANCED_FACE ( 'NONE', ( #4919 ), #4053, .F. ) ;
#5093 = DIRECTION ( 'NONE',  ( -1.000000000000000000, 0.000000000000000000, -7.228014483236656373E-17 ) ) ;
#5094 = ORIENTED_EDGE ( 'NONE', *, *, #3687, .F. ) ;
#5095 = CARTESIAN_POINT ( 'NONE',  ( -344.8278606858024204, 3.635192770030907673E-30, 239.0993754495075621 ) ) ;
#5096 = CARTESIAN_POINT ( 'NONE',  ( -198.3455225866217404, 1.517883041479706208E-15, 518.3576047634792303 ) ) ;
#5097 = DIRECTION ( 'NONE',  ( -1.000000000000000000, 0.000000000000000000, 0.000000000000000000 ) ) ;
#5098 = VERTEX_POINT ( 'NONE', #3179 ) ;
#5099 = TOROIDAL_SURFACE ( 'NONE', #102, 28.50000000000115463, 1.000000000000000000 ) ;
#5100 = EDGE_LOOP ( 'NONE', ( #945, #2345 ) ) ;
#5101 = LINE ( 'NONE', #4707, #509 ) ;
#5102 =( LENGTH_UNIT ( ) NAMED_UNIT ( * ) SI_UNIT ( .MILLI., .METRE. ) );
#5103 = EDGE_CURVE ( 'NONE', #783, #1799, #3645, .T. ) ;
#5104 = VECTOR ( 'NONE', #4408, 1000.000000000000000 ) ;
#5105 = EDGE_CURVE ( 'NONE', #3075, #467, #3019, .T. ) ;
#5106 = VERTEX_POINT ( 'NONE', #3568 ) ;
#5107 = CARTESIAN_POINT ( 'NONE',  ( 36.66581985038869362, 3.252606517456513302E-16, 340.1662229844753256 ) ) ;
#5108 = ORIENTED_EDGE ( 'NONE', *, *, #4853, .T. ) ;
#5109 = CARTESIAN_POINT ( 'NONE',  ( -315.6465677682754176, 5.957787190994864669E-15, 121.3180010999883791 ) ) ;
#5110 = CARTESIAN_POINT ( 'NONE',  ( -312.0566616799260373, -25.00000000000003197, 419.2731246273838792 ) ) ;
#5111 = CIRCLE ( 'NONE', #380, 6.000000000000032863 ) ;
#5112 = VECTOR ( 'NONE', #4549, 1000.000000000000114 ) ;
#5113 = LINE ( 'NONE', #3065, #3363 ) ;
#5114 = DIRECTION ( 'NONE',  ( 5.551115123125772841E-17, -1.848892746611743135E-31, -1.000000000000000000 ) ) ;
#5115 = AXIS2_PLACEMENT_3D ( 'NONE', #2953, #1735, #3773 ) ;
#5116 = ORIENTED_EDGE ( 'NONE', *, *, #4654, .T. ) ;
#5117 = ORIENTED_EDGE ( 'NONE', *, *, #3117, .F. ) ;
#5118 = EDGE_LOOP ( 'NONE', ( #1098, #579, #3813, #1276 ) ) ;
#5119 = LINE ( 'NONE', #4359, #3384 ) ;
#5120 = DIRECTION ( 'NONE',  ( -0.9955873536034883786, 5.497582812564159916E-31, -0.09383933793885515517 ) ) ;
#5121 = CARTESIAN_POINT ( 'NONE',  ( -353.4921497144319460, 2.222614453595284090E-15, 38.40071206960160310 ) ) ;
#5122 = AXIS2_PLACEMENT_3D ( 'NONE', #3123, #998, #943 ) ;
#5123 = EDGE_CURVE ( 'NONE', #864, #1607, #3618, .T. ) ;
#5124 = VECTOR ( 'NONE', #473, 1000.000000000000000 ) ;
#5125 = FACE_OUTER_BOUND ( 'NONE', #1675, .T. ) ;
#5126 = EDGE_LOOP ( 'NONE', ( #1740, #1869, #4974, #3786 ) ) ;
#5127 = CIRCLE ( 'NONE', #1181, 22.67218956682437536 ) ;
#5128 = CIRCLE ( 'NONE', #2762, 31.50000000000120082 ) ;
#5129 = CARTESIAN_POINT ( 'NONE',  ( -48.13570084519473369, 15.00000000000001421, 62.68703548022111249 ) ) ;
#5130 = CARTESIAN_POINT ( 'NONE',  ( -14.89480152442229688, 0.000000000000000000, 508.6517828409968729 ) ) ;
#5131 =( GEOMETRIC_REPRESENTATION_CONTEXT ( 3 ) GLOBAL_UNCERTAINTY_ASSIGNED_CONTEXT ( ( #5170 ) ) GLOBAL_UNIT_ASSIGNED_CONTEXT ( ( #5079, #3427, #1888 ) ) REPRESENTATION_CONTEXT ( 'NONE', 'WORKASPACE' ) );
#5132 = LINE ( 'NONE', #650, #1797 ) ;
#5133 = APPLICATION_CONTEXT ( 'automotive_design' ) ;
#5134 = EDGE_LOOP ( 'NONE', ( #198, #5146, #1721, #4305 ) ) ;
#5135 = DIRECTION ( 'NONE',  ( 5.551115123125772841E-17, -1.848892746611743135E-31, -1.000000000000000000 ) ) ;
#5136 = LINE ( 'NONE', #3031, #2088 ) ;
#5137 = EDGE_LOOP ( 'NONE', ( #1048, #3132, #1275, #712 ) ) ;
#5138 = CARTESIAN_POINT ( 'NONE',  ( -367.0882437885061904, 2.222614453595284090E-15, 297.8351940652699454 ) ) ;
#5139 = ORIENTED_EDGE ( 'NONE', *, *, #1030, .T. ) ;
#5140 = DIRECTION ( 'NONE',  ( 5.551115123125772841E-17, -1.848892746611743135E-31, -1.000000000000000000 ) ) ;
#5141 = ADVANCED_FACE ( 'NONE', ( #5226 ), #1992, .F. ) ;
#5142 = CARTESIAN_POINT ( 'NONE',  ( -63.04765821500757284, -24.99999999999981881, 521.0401840782880072 ) ) ;
#5143 = CARTESIAN_POINT ( 'NONE',  ( 139.9714219172562650, -21.54565493204319182, -2.000000000000001332 ) ) ;
#5144 = CARTESIAN_POINT ( 'NONE',  ( 137.9714219172561229, -39.54565493204319182, 152.0000000000004263 ) ) ;
#5145 = ORIENTED_EDGE ( 'NONE', *, *, #2585, .F. ) ;
#5146 = ORIENTED_EDGE ( 'NONE', *, *, #2765, .T. ) ;
#5147 = VERTEX_POINT ( 'NONE', #317 ) ;
#5148 = CARTESIAN_POINT ( 'NONE',  ( -0.6802310551622114954, 2.222614453595284090E-15, 47.14310755735262859 ) ) ;
#5149 = DIRECTION ( 'NONE',  ( -0.9955873536034882676, 5.498529991225532086E-31, -0.09383933793885536334 ) ) ;
#5150 = DIRECTION ( 'NONE',  ( 0.9955873536034882676, -5.273458392682099492E-31, 0.09383933793885600172 ) ) ;
#5151 = AXIS2_PLACEMENT_3D ( 'NONE', #4931, #647, #1913 ) ;
#5152 = ORIENTED_EDGE ( 'NONE', *, *, #2944, .T. ) ;
#5153 = AXIS2_PLACEMENT_3D ( 'NONE', #2612, #1855, #3542 ) ;
#5154 = DIRECTION ( 'NONE',  ( -5.720779902258401340E-31, -1.000000000000000000, 2.099398147291833041E-31 ) ) ;
#5155 = CARTESIAN_POINT ( 'NONE',  ( 24.85474708473260108, -25.00000000000000355, 216.1905617304888665 ) ) ;
#5156 = DIRECTION ( 'NONE',  ( 0.000000000000000000, 0.000000000000000000, 1.000000000000000000 ) ) ;
#5157 = CIRCLE ( 'NONE', #1383, 22.67218956682437536 ) ;
#5158 = EDGE_CURVE ( 'NONE', #1066, #4519, #5378, .T. ) ;
#5159 = ORIENTED_EDGE ( 'NONE', *, *, #2208, .F. ) ;
#5160 = CARTESIAN_POINT ( 'NONE',  ( -122.4270646331731598, 3.252606517456513302E-16, 560.5113017241549187 ) ) ;
#5161 = DIRECTION ( 'NONE',  ( 1.000000000000000000, 0.000000000000000000, 0.000000000000000000 ) ) ;
#5162 = EDGE_CURVE ( 'NONE', #467, #4218, #3592, .T. ) ;
#5163 = ORIENTED_EDGE ( 'NONE', *, *, #894, .F. ) ;
#5164 = CARTESIAN_POINT ( 'NONE',  ( -72.60637664584184847, 3.252606517456513302E-16, 552.9197695054128872 ) ) ;
#5165 = ORIENTED_EDGE ( 'NONE', *, *, #2496, .F. ) ;
#5166 = LINE ( 'NONE', #1432, #4162 ) ;
#5167 = CARTESIAN_POINT ( 'NONE',  ( 139.2214219172562650, -21.54565493204319182, -12.00000000000006573 ) ) ;
#5168 = DIRECTION ( 'NONE',  ( -1.000000000000000000, 0.000000000000000000, -5.551115123125777155E-17 ) ) ;
#5169 = EDGE_LOOP ( 'NONE', ( #3030, #3029 ) ) ;
#5170 = UNCERTAINTY_MEASURE_WITH_UNIT (LENGTH_MEASURE( 1.000000000000000082E-05 ), #5079, 'distance_accuracy_value', 'NONE');
#5171 = VERTEX_POINT ( 'NONE', #1137 ) ;
#5172 = PLANE ( 'NONE',  #3816 ) ;
#5173 = DIRECTION ( 'NONE',  ( 5.551115123125772841E-17, -1.848892746611743135E-31, -1.000000000000000000 ) ) ;
#5174 = DIRECTION ( 'NONE',  ( -0.000000000000000000, -1.000000000000000000, -0.000000000000000000 ) ) ;
#5175 = EDGE_CURVE ( 'NONE', #4078, #3769, #3213, .T. ) ;
#5176 = PRESENTATION_STYLE_ASSIGNMENT (( #4797 ) ) ;
#5177 = ORIENTED_EDGE ( 'NONE', *, *, #3887, .F. ) ;
#5178 = DIRECTION ( 'NONE',  ( 0.09383933793885537722, -2.626968444144180508E-31, -0.9955873536034883786 ) ) ;
#5179 = CARTESIAN_POINT ( 'NONE',  ( -207.8397519515722252, -25.00000000000003197, 541.5412455041529256 ) ) ;
#5180 = CARTESIAN_POINT ( 'NONE',  ( 137.9714219172561798, -39.54565493204318471, -5.551115123125782702E-14 ) ) ;
#5181 = CARTESIAN_POINT ( 'NONE',  ( -108.3530091724271358, 0.000000000000000000, 123.8676211295743599 ) ) ;
#5182 = CARTESIAN_POINT ( 'NONE',  ( -360.7307227603793649, 2.222614453595284090E-15, 354.4373729494858480 ) ) ;
#5183 = PRODUCT_CONTEXT ( 'NONE', #5133, 'mechanical' ) ;
#5184 = EDGE_CURVE ( 'NONE', #179, #1676, #2403, .T. ) ;
#5185 = ORIENTED_EDGE ( 'NONE', *, *, #4694, .F. ) ;
#5186 = CARTESIAN_POINT ( 'NONE',  ( -30.63277980166709114, 25.00000000000018474, 527.1358351633700750 ) ) ;
#5187 = ORIENTED_EDGE ( 'NONE', *, *, #3507, .T. ) ;
#5188 = EDGE_CURVE ( 'NONE', #4435, #3915, #635, .T. ) ;
#5189 = EDGE_CURVE ( 'NONE', #1486, #2971, #4003, .T. ) ;
#5190 = DIRECTION ( 'NONE',  ( -0.9955873536034882676, 5.502656983963203831E-31, -0.09383933793885550212 ) ) ;
#5191 = PLANE ( 'NONE',  #5122 ) ;
#5192 = AXIS2_PLACEMENT_3D ( 'NONE', #5313, #2405, #752 ) ;
#5193 = ORIENTED_EDGE ( 'NONE', *, *, #5330, .T. ) ;
#5194 = CIRCLE ( 'NONE', #5282, 21.00000000000124700 ) ;
#5195 = CIRCLE ( 'NONE', #5289, 5.250000000000018652 ) ;
#5196 = EDGE_LOOP ( 'NONE', ( #2097, #1750 ) ) ;
#5197 = CARTESIAN_POINT ( 'NONE',  ( -78.28422483266231779, -26.49739520581859153, -10.00000000000006395 ) ) ;
#5198 = DIRECTION ( 'NONE',  ( -0.09383933793885568253, 2.673190762809473730E-31, 0.9955873536034882676 ) ) ;
#5199 = DIRECTION ( 'NONE',  ( -1.000000000000000000, 0.000000000000000000, -7.228014483236656373E-17 ) ) ;
#5200 =( REPRESENTATION_RELATIONSHIP ('NONE','NONE', #2124, #825 ) REPRESENTATION_RELATIONSHIP_WITH_TRANSFORMATION ( #679 )SHAPE_REPRESENTATION_RELATIONSHIP( ) );
#5201 = VECTOR ( 'NONE', #1367, 1000.000000000000114 ) ;
#5202 = AXIS2_PLACEMENT_3D ( 'NONE', #1584, #3308, #329 ) ;
#5203 =( LENGTH_UNIT ( ) NAMED_UNIT ( * ) SI_UNIT ( .MILLI., .METRE. ) );
#5204 = ORIENTED_EDGE ( 'NONE', *, *, #3783, .F. ) ;
#5205 = COLOUR_RGB ( '',0.7921568627450980005, 0.8196078431372548767, 0.9333333333333333481 ) ;
#5206 = CARTESIAN_POINT ( 'NONE',  ( -345.9181427152443007, 2.222614453595284090E-15, 117.4603139392499429 ) ) ;
#5207 = AXIS2_PLACEMENT_3D ( 'NONE', #696, #589, #2379 ) ;
#5208 = CARTESIAN_POINT ( 'NONE',  ( -105.2090356704102447, -24.99999999999981881, 560.1816718768288865 ) ) ;
#5209 = CARTESIAN_POINT ( 'NONE',  ( 96.73877717791896202, -14.99999999999998579, 131.6034880481681171 ) ) ;
#5210 = DIRECTION ( 'NONE',  ( -0.9072577839912278064, 0.4205749795070158892, 5.551115123125773458E-17 ) ) ;
#5211 = VECTOR ( 'NONE', #1559, 1000.000000000000227 ) ;
#5212 = TOROIDAL_SURFACE ( 'NONE', #1533, 30.50000000000105516, 1.000000000000000000 ) ;
#5213 = ORIENTED_EDGE ( 'NONE', *, *, #3823, .F. ) ;
#5214 = CARTESIAN_POINT ( 'NONE',  ( -105.2090356704105147, 2.222614453595284090E-15, 560.1816718768288865 ) ) ;
#5215 = CARTESIAN_POINT ( 'NONE',  ( 29.23877717791895847, -9.038641713901924390, 67.09613410133256650 ) ) ;
#5216 = CIRCLE ( 'NONE', #2400, 49.99999999999996447 ) ;
#5217 = ORIENTED_EDGE ( 'NONE', *, *, #1736, .F. ) ;
#5218 = CARTESIAN_POINT ( 'NONE',  ( 24.85474708473287109, 3.252606517456513302E-16, 216.1905617304896623 ) ) ;
#5219 = EDGE_CURVE ( 'NONE', #3515, #3069, #2838, .T. ) ;
#5220 = ORIENTED_EDGE ( 'NONE', *, *, #2234, .T. ) ;
#5221 = CARTESIAN_POINT ( 'NONE',  ( -80.02857808274410445, -21.54565493204320248, -26.84924240491759662 ) ) ;
#5222 = DIRECTION ( 'NONE',  ( 1.000000000000000000, 0.000000000000000000, 0.000000000000000000 ) ) ;
#5223 = ORIENTED_EDGE ( 'NONE', *, *, #3615, .T. ) ;
#5224 = PRODUCT_DEFINITION_CONTEXT ( 'detailed design', #815, 'design' ) ;
#5225 = ORIENTED_EDGE ( 'NONE', *, *, #1436, .F. ) ;
#5226 = FACE_OUTER_BOUND ( 'NONE', #1328, .T. ) ;
#5227 = CARTESIAN_POINT ( 'NONE',  ( -80.02857808274410445, -21.54565493204321669, -9.999999999999953815 ) ) ;
#5228 = EDGE_CURVE ( 'NONE', #2780, #1607, #260, .T. ) ;
#5229 = CARTESIAN_POINT ( 'NONE',  ( -330.6206199554102341, 2.816687638039051980E-15, 200.2611943537262107 ) ) ;
#5230 = PLANE ( 'NONE',  #4961 ) ;
#5231 = DIRECTION ( 'NONE',  ( 1.000000000000000000, 0.000000000000000000, 0.000000000000000000 ) ) ;
#5232 = ORIENTED_EDGE ( 'NONE', *, *, #3328, .T. ) ;
#5233 = FACE_OUTER_BOUND ( 'NONE', #4358, .T. ) ;
#5234 = CARTESIAN_POINT ( 'NONE',  ( 16.26935751051944479, 3.252606517456513302E-16, 140.3055424402290896 ) ) ;
#5235 = DIRECTION ( 'NONE',  ( -5.551115123125772841E-17, 1.848892746611743135E-31, 1.000000000000000000 ) ) ;
#5236 = CARTESIAN_POINT ( 'NONE',  ( -80.02857808274401918, 80.45434506795689344, -12.00000000000001066 ) ) ;
#5237 = DIRECTION ( 'NONE',  ( -0.09383933793885568253, 2.673190762809473730E-31, 0.9955873536034882676 ) ) ;
#5238 = CARTESIAN_POINT ( 'NONE',  ( 18.31346110193259946, 25.00000000000018474, 444.2932575970297648 ) ) ;
#5239 = DIRECTION ( 'NONE',  ( 0.9393298923196348182, 0.000000000000000000, -0.3430150920801929293 ) ) ;
#5240 = CARTESIAN_POINT ( 'NONE',  ( 34.60640066538617532, -24.99999999999981881, 295.6817845355782879 ) ) ;
#5241 = AXIS2_PLACEMENT_3D ( 'NONE', #2738, #4421, #2330 ) ;
#5242 = EDGE_LOOP ( 'NONE', ( #3244, #98, #2189, #4901 ) ) ;
#5243 = CARTESIAN_POINT ( 'NONE',  ( 6.585909452853061730, 3.740497495074990297E-15, 393.9228865916071527 ) ) ;
#5244 = VERTEX_POINT ( 'NONE', #1931 ) ;
#5245 = DIRECTION ( 'NONE',  ( 5.551115123125772841E-17, -1.848892746611743135E-31, -1.000000000000000000 ) ) ;
#5246 = DIRECTION ( 'NONE',  ( -1.219242865862094703E-16, 1.000000000000000000, -1.149200448409289593E-17 ) ) ;
#5247 = ORIENTED_EDGE ( 'NONE', *, *, #4630, .F. ) ;
#5248 = ORIENTED_EDGE ( 'NONE', *, *, #5308, .F. ) ;
#5249 = LINE ( 'NONE', #1488, #197 ) ;
#5250 = DIRECTION ( 'NONE',  ( 5.551115123125772841E-17, -1.848892746611743135E-31, -1.000000000000000000 ) ) ;
#5251 = CARTESIAN_POINT ( 'NONE',  ( 136.6230329513292361, -17.01448963777488288, -9.999999999999953815 ) ) ;
#5252 = DIRECTION ( 'NONE',  ( 5.551115123125772841E-17, -1.848892746611743354E-31, -1.000000000000000000 ) ) ;
#5253 = ADVANCED_FACE ( 'NONE', ( #4813 ), #1162, .T. ) ;
#5254 = LINE ( 'NONE', #3156, #1177 ) ;
#5255 = ORIENTED_EDGE ( 'NONE', *, *, #3631, .T. ) ;
#5256 = EDGE_CURVE ( 'NONE', #2877, #281, #4417, .T. ) ;
#5257 = EDGE_CURVE ( 'NONE', #4186, #1654, #5249, .T. ) ;
#5258 = CARTESIAN_POINT ( 'NONE',  ( -344.1351952944061168, 5.421010862427522170E-17, 98.54415422078321285 ) ) ;
#5259 = EDGE_CURVE ( 'NONE', #179, #534, #3375, .T. ) ;
#5260 = DIRECTION ( 'NONE',  ( 0.000000000000000000, 1.000000000000000000, 0.000000000000000000 ) ) ;
#5261 = DIRECTION ( 'NONE',  ( -0.9955873536034883786, 5.497582812564159916E-31, -0.09383933793885515517 ) ) ;
#5262 = DIRECTION ( 'NONE',  ( -0.9955873536034881566, 5.462637660443544243E-31, -0.09383933793885600172 ) ) ;
#5263 = DIRECTION ( 'NONE',  ( 0.000000000000000000, -1.000000000000000000, 0.000000000000000000 ) ) ;
#5264 = CARTESIAN_POINT ( 'NONE',  ( -223.9642223310785312, 5.421010862427522170E-17, 534.3227077389987016 ) ) ;
#5265 = CARTESIAN_POINT ( 'NONE',  ( -213.0979982360503584, 1.517883041479706208E-15, 511.7519955242227070 ) ) ;
#5266 = CARTESIAN_POINT ( 'NONE',  ( -377.1442077948352107, 5.590393151250686046E-15, 155.6988136436743559 ) ) ;
#5267 = ORIENTED_EDGE ( 'NONE', *, *, #1604, .F. ) ;
#5268 = CARTESIAN_POINT ( 'NONE',  ( -35.15684241565268309, 25.00000000000018474, 493.9702760599490716 ) ) ;
#5269 = EDGE_LOOP ( 'NONE', ( #152, #5071, #5232, #4121 ) ) ;
#5270 = DIRECTION ( 'NONE',  ( -0.01527226085271972227, -2.080004339938201146E-31, -0.9998833722232041143 ) ) ;
#5271 = EDGE_CURVE ( 'NONE', #3541, #3680, #818, .T. ) ;
#5272 = VECTOR ( 'NONE', #3863, 1000.000000000000000 ) ;
#5273 = ORIENTED_EDGE ( 'NONE', *, *, #4229, .F. ) ;
#5274 = ORIENTED_EDGE ( 'NONE', *, *, #1471, .F. ) ;
#5275 = DIRECTION ( 'NONE',  ( 5.551115123125772841E-17, -1.848892746611743135E-31, -1.000000000000000000 ) ) ;
#5276 = AXIS2_PLACEMENT_3D ( 'NONE', #1933, #4468, #4030 ) ;
#5277 = DIRECTION ( 'NONE',  ( 1.000000000000000000, 0.000000000000000000, 0.000000000000000000 ) ) ;
#5278 = DIRECTION ( 'NONE',  ( -0.09383933793885568253, 2.673190762809473730E-31, 0.9955873536034882676 ) ) ;
#5279 = PLANE ( 'NONE',  #3107 ) ;
#5280 =( NAMED_UNIT ( * ) SI_UNIT ( $, .STERADIAN. ) SOLID_ANGLE_UNIT ( ) );
#5281 = VERTEX_POINT ( 'NONE', #4599 ) ;
#5282 = AXIS2_PLACEMENT_3D ( 'NONE', #253, #1872, #5190 ) ;
#5283 = EDGE_CURVE ( 'NONE', #1569, #994, #5195, .T. ) ;
#5284 = DIRECTION ( 'NONE',  ( -1.000000000000000000, 3.759415251443877379E-31, -5.551115123125772841E-17 ) ) ;
#5285 = DIRECTION ( 'NONE',  ( 0.09383933793885537722, -2.626968444144180508E-31, -0.9955873536034883786 ) ) ;
#5286 = FACE_OUTER_BOUND ( 'NONE', #1106, .T. ) ;
#5287 = CARTESIAN_POINT ( 'NONE',  ( -0.8482259245422840710, 2.276824562219559311E-15, 36.14439046289818691 ) ) ;
#5288 = AXIS2_PLACEMENT_3D ( 'NONE', #5236, #2691, #2329 ) ;
#5289 = AXIS2_PLACEMENT_3D ( 'NONE', #1218, #3751, #3343 ) ;
#5290 = DIRECTION ( 'NONE',  ( -5.551115123125772841E-17, 1.848892746611743135E-31, 1.000000000000000000 ) ) ;
#5291 = CIRCLE ( 'NONE', #1790, 28.50000000000127898 ) ;
#5292 = VECTOR ( 'NONE', #3658, 1000.000000000000000 ) ;
#5293 = CYLINDRICAL_SURFACE ( 'NONE', #252, 5.250000000000004441 ) ;
#5294 = CARTESIAN_POINT ( 'NONE',  ( -320.6447527397745034, 24.99999999999997158, 453.8399743637903612 ) ) ;
#5295 = CARTESIAN_POINT ( 'NONE',  ( 36.66581985038869362, 3.252606517456513302E-16, 340.1662229844753256 ) ) ;
#5296 = DIRECTION ( 'NONE',  ( -5.551115123125772841E-17, 1.848892746611743135E-31, 1.000000000000000000 ) ) ;
#5297 = AXIS2_PLACEMENT_3D ( 'NONE', #2091, #4238, #3768 ) ;
#5298 = AXIS2_PLACEMENT_3D ( 'NONE', #2763, #1851, #3540 ) ;
#5299 = CIRCLE ( 'NONE', #4261, 17.00000000000009948 ) ;
#5300 = VERTEX_POINT ( 'NONE', #4214 ) ;
#5301 = CARTESIAN_POINT ( 'NONE',  ( -336.1069982926114221, 25.00000000000018474, 349.6877309229307684 ) ) ;
#5302 = PRODUCT_DEFINITION_SHAPE ( 'NONE', 'NONE',  #5434 ) ;
#5303 = EDGE_LOOP ( 'NONE', ( #1801, #3967, #2994, #938 ) ) ;
#5304 = CIRCLE ( 'NONE', #42, 56.63911695420845405 ) ;
#5305 = DIRECTION ( 'NONE',  ( 5.551115123125772841E-17, -1.848892746611743135E-31, -1.000000000000000000 ) ) ;
#5306 = CARTESIAN_POINT ( 'NONE',  ( -81.77293133282597637, -16.59391465826784540, -10.00000000000000888 ) ) ;
#5307 = EDGE_LOOP ( 'NONE', ( #2535, #4008 ) ) ;
#5308 = EDGE_CURVE ( 'NONE', #3702, #744, #836, .T. ) ;
#5309 =( GEOMETRIC_REPRESENTATION_CONTEXT ( 3 ) GLOBAL_UNCERTAINTY_ASSIGNED_CONTEXT ( ( #4895 ) ) GLOBAL_UNIT_ASSIGNED_CONTEXT ( ( #1289, #3033, #4348 ) ) REPRESENTATION_CONTEXT ( 'NONE', 'WORKASPACE' ) );
#5310 = EDGE_LOOP ( 'NONE', ( #1302, #5087, #3756, #4083 ) ) ;
#5311 = CARTESIAN_POINT ( 'NONE',  ( 137.9714219172562650, 84.45434506795687923, -5.551115123125782702E-14 ) ) ;
#5312 = DIRECTION ( 'NONE',  ( 0.000000000000000000, 0.000000000000000000, 1.000000000000000000 ) ) ;
#5313 = CARTESIAN_POINT ( 'NONE',  ( -353.4252897503525332, 0.000000000000000000, 197.1073022275279243 ) ) ;
#5314 = DIRECTION ( 'NONE',  ( -1.000000000000000000, 3.759415251443877379E-31, -5.551115123125772841E-17 ) ) ;
#5315 = DIRECTION ( 'NONE',  ( 5.551115123125772841E-17, -1.848892746611743135E-31, -1.000000000000000000 ) ) ;
#5316 = EDGE_LOOP ( 'NONE', ( #1075, #120, #3118, #2621 ) ) ;
#5317 = SURFACE_STYLE_FILL_AREA ( #2729 ) ;
#5318 = DIRECTION ( 'NONE',  ( 0.9955873536034882676, -5.498835694391114214E-31, 0.09383933793885514130 ) ) ;
#5319 = DIRECTION ( 'NONE',  ( -0.09383933793885568253, 2.673190762809473730E-31, 0.9955873536034882676 ) ) ;
#5320 = CARTESIAN_POINT ( 'NONE',  ( -351.5485029915759583, 2.222614453595284090E-15, 177.1955551554592603 ) ) ;
#5321 = FACE_OUTER_BOUND ( 'NONE', #3622, .T. ) ;
#5322 = DIRECTION ( 'NONE',  ( -5.551115123125772841E-17, 1.848892746611743354E-31, 1.000000000000000000 ) ) ;
#5323 = CARTESIAN_POINT ( 'NONE',  ( -167.9289969670495282, 25.00000000000018474, 528.5729890193230176 ) ) ;
#5324 = CARTESIAN_POINT ( 'NONE',  ( -14.89480152442229688, 0.000000000000000000, 508.6517828409968729 ) ) ;
#5325 = ORIENTED_EDGE ( 'NONE', *, *, #1206, .T. ) ;
#5326 = CARTESIAN_POINT ( 'NONE',  ( -12.39202333278750601, 25.00000000000000355, 98.84296066633362443 ) ) ;
#5327 = ORIENTED_EDGE ( 'NONE', *, *, #1221, .F. ) ;
#5328 = ADVANCED_FACE ( 'NONE', ( #5001 ), #3697, .T. ) ;
#5329 = TOROIDAL_SURFACE ( 'NONE', #1294, 30.50000000000105516, 1.000000000000000000 ) ;
#5330 = EDGE_CURVE ( 'NONE', #2627, #4404, #2537, .T. ) ;
#5331 = VECTOR ( 'NONE', #136, 1000.000000000000114 ) ;
#5332 = CARTESIAN_POINT ( 'NONE',  ( -346.0119820531829191, 0.000000000000000000, 118.4559012928527721 ) ) ;
#5333 = EDGE_CURVE ( 'NONE', #1369, #5147, #856, .T. ) ;
#5334 = DIRECTION ( 'NONE',  ( 0.000000000000000000, 0.000000000000000000, 1.000000000000000000 ) ) ;
#5335 = AXIS2_PLACEMENT_3D ( 'NONE', #1528, #2795, #4560 ) ;
#5336 = ORIENTED_EDGE ( 'NONE', *, *, #2519, .F. ) ;
#5337 = PRODUCT_DEFINITION_CONTEXT ( 'detailed design', #5411, 'design' ) ;
#5338 = ORIENTED_EDGE ( 'NONE', *, *, #4380, .F. ) ;
#5339 = CARTESIAN_POINT ( 'NONE',  ( -80.02857808274418971, -21.54565493204321669, -2.000000000000001776 ) ) ;
#5340 = DIRECTION ( 'NONE',  ( -0.09383933793885537722, 2.626968444144180508E-31, 0.9955873536034883786 ) ) ;
#5341 = VECTOR ( 'NONE', #3742, 1000.000000000000114 ) ;
#5342 = LINE ( 'NONE', #4055, #2043 ) ;
#5343 = CARTESIAN_POINT ( 'NONE',  ( -357.2727026058461206, 5.421010862427522170E-17, 237.9263837252718758 ) ) ;
#5344 = LINE ( 'NONE', #440, #1616 ) ;
#5345 = EDGE_LOOP ( 'NONE', ( #2467, #3482 ) ) ;
#5346 = CARTESIAN_POINT ( 'NONE',  ( 133.9714219172562366, -21.54565493204323090, -9.999999999999841904 ) ) ;
#5347 = CARTESIAN_POINT ( 'NONE',  ( -85.27857808274410445, -21.54565493204320248, -12.00000000000001066 ) ) ;
#5348 = CARTESIAN_POINT ( 'NONE',  ( 151.9714219172562650, -25.54565493204307813, -11.99999999999995559 ) ) ;
#5349 = CARTESIAN_POINT ( 'NONE',  ( 0.000000000000000000, 80.00000000000000000, 0.000000000000000000 ) ) ;
#5350 = ADVANCED_FACE ( 'NONE', ( #2895 ), #443, .T. ) ;
#5351 = CARTESIAN_POINT ( 'NONE',  ( 133.9714219172562366, -21.54565493204319182, -2.000000000000001776 ) ) ;
#5352 = CARTESIAN_POINT ( 'NONE',  ( -156.9923520473274721, 25.00000000000018474, 556.8176423728723421 ) ) ;
#5353 = CARTESIAN_POINT ( 'NONE',  ( 29.77542608467492613, 2.222614453595284090E-15, 249.2409987768030533 ) ) ;
#5354 = ORIENTED_EDGE ( 'NONE', *, *, #5105, .F. ) ;
#5355 = CARTESIAN_POINT ( 'NONE',  ( -48.20943979671786650, 25.00000000000018474, 509.2978244404892507 ) ) ;
#5356 = ORIENTED_EDGE ( 'NONE', *, *, #2341, .T. ) ;
#5357 = DIRECTION ( 'NONE',  ( 0.09383933793885568253, -2.673190762809473730E-31, -0.9955873536034882676 ) ) ;
#5358 = EDGE_CURVE ( 'NONE', #251, #1398, #1239, .T. ) ;
#5359 = DIRECTION ( 'NONE',  ( 0.000000000000000000, -1.000000000000000000, 0.000000000000000000 ) ) ;
#5360 = ORIENTED_EDGE ( 'NONE', *, *, #960, .F. ) ;
#5361 = ADVANCED_FACE ( 'NONE', ( #2461 ), #4163, .F. ) ;
#5362 = ORIENTED_EDGE ( 'NONE', *, *, #111, .T. ) ;
#5363 = CARTESIAN_POINT ( 'NONE',  ( -338.5986743560152377, -14.95948628165117178, 39.80450035817695209 ) ) ;
#5364 = CARTESIAN_POINT ( 'NONE',  ( -323.0598754654449181, 3.735172737399573480E-15, 199.9694020346631191 ) ) ;
#5365 = LINE ( 'NONE', #1194, #4499 ) ;
#5366 = CARTESIAN_POINT ( 'NONE',  ( -369.7175445258896502, 1.530808498934214793E-15, 236.7533920010361896 ) ) ;
#5367 = DIRECTION ( 'NONE',  ( -1.000000000000000000, 0.000000000000000000, 0.000000000000000000 ) ) ;
#5368 = VERTEX_POINT ( 'NONE', #4957 ) ;
#5369 = AXIS2_PLACEMENT_3D ( 'NONE', #149, #4384, #2246 ) ;
#5370 = ORIENTED_EDGE ( 'NONE', *, *, #2816, .T. ) ;
#5371 = CARTESIAN_POINT ( 'NONE',  ( -84.02857808274413287, 84.45434506795682239, 152.0000000000003126 ) ) ;
#5372 = CARTESIAN_POINT ( 'NONE',  ( 96.73877717791896202, -14.99999999999998579, 67.09613410133256650 ) ) ;
#5373 = CARTESIAN_POINT ( 'NONE',  ( -321.8445680969931004, 4.999156891862629509E-15, 103.6584595401686215 ) ) ;
#5374 = AXIS2_PLACEMENT_3D ( 'NONE', #201, #2726, #3181 ) ;
#5375 = DIRECTION ( 'NONE',  ( -0.09383933793885537722, 2.626968444144180508E-31, 0.9955873536034883786 ) ) ;
#5376 = AXIS2_PLACEMENT_3D ( 'NONE', #5077, #1703, #1321 ) ;
#5377 = DIRECTION ( 'NONE',  ( 0.000000000000000000, 0.000000000000000000, 1.000000000000000000 ) ) ;
#5378 = CIRCLE ( 'NONE', #4850, 6.000000000000032863 ) ;
#5379 = CARTESIAN_POINT ( 'NONE',  ( 0.07030049710132768581, 1.843143693225357538E-15, 219.5055207296747710 ) ) ;
#5380 = ITEM_DEFINED_TRANSFORMATION ( 'NONE', 'NONE', #220,  #2926 ) ;
#5381 = CARTESIAN_POINT ( 'NONE',  ( -320.6447527397726276, 2.276824562219559311E-15, 453.8399743637901906 ) ) ;
#5382 = AXIS2_PLACEMENT_3D ( 'NONE', #2960, #3050, #4227 ) ;
#5383 = EDGE_LOOP ( 'NONE', ( #3921, #2215, #1828, #3177 ) ) ;
#5384 = ORIENTED_EDGE ( 'NONE', *, *, #4460, .T. ) ;
#5385 = DIRECTION ( 'NONE',  ( 5.551115123125772841E-17, -1.848892746611743135E-31, -1.000000000000000000 ) ) ;
#5386 = CIRCLE ( 'NONE', #3027, 5.250000000000018652 ) ;
#5387 =( NAMED_UNIT ( * ) PLANE_ANGLE_UNIT ( ) SI_UNIT ( $, .RADIAN. ) );
#5388 = ORIENTED_EDGE ( 'NONE', *, *, #2878, .T. ) ;
#5389 = CIRCLE ( 'NONE', #3388, 5.250000000000031974 ) ;
#5390 = AXIS2_PLACEMENT_3D ( 'NONE', #1768, #2653, #562 ) ;
#5391 = PRODUCT_DEFINITION_SHAPE ( 'NONE', 'NONE',  #3211 ) ;
#5392 = DIRECTION ( 'NONE',  ( 0.000000000000000000, -1.000000000000000000, 0.000000000000000000 ) ) ;
#5393 = CARTESIAN_POINT ( 'NONE',  ( -323.7051989975983588, 2.222614453595284090E-15, 41.20828864675230108 ) ) ;
#5394 = DIRECTION ( 'NONE',  ( -5.551115123125772841E-17, 1.848892746611743354E-31, 1.000000000000000000 ) ) ;
#5395 = FACE_OUTER_BOUND ( 'NONE', #1997, .T. ) ;
#5396 =( GEOMETRIC_REPRESENTATION_CONTEXT ( 3 ) GLOBAL_UNCERTAINTY_ASSIGNED_CONTEXT ( ( #2809 ) ) GLOBAL_UNIT_ASSIGNED_CONTEXT ( ( #988, #4319, #165 ) ) REPRESENTATION_CONTEXT ( 'NONE', 'WORKASPACE' ) );
#5397 = VERTEX_POINT ( 'NONE', #2513 ) ;
#5398 = EDGE_CURVE ( 'NONE', #1369, #2476, #2491, .T. ) ;
#5399 = CIRCLE ( 'NONE', #3043, 17.00000000000009948 ) ;
#5400 = VERTEX_POINT ( 'NONE', #1269 ) ;
#5401 = LINE ( 'NONE', #4636, #2238 ) ;
#5402 = CARTESIAN_POINT ( 'NONE',  ( -80.02857808274413287, 80.45434506795689344, -26.84924240491753977 ) ) ;
#5403 = CARTESIAN_POINT ( 'NONE',  ( -319.3419943896644213, 2.222614453595281723E-15, 41.61954360114513207 ) ) ;
#5404 = DIRECTION ( 'NONE',  ( 5.551115123125772841E-17, -1.848892746611743135E-31, -1.000000000000000000 ) ) ;
#5405 = CARTESIAN_POINT ( 'NONE',  ( -52.92425795464261995, 3.794707603699265519E-15, 513.6488213284153517 ) ) ;
#5406 = CARTESIAN_POINT ( 'NONE',  ( -367.0882437885064746, 25.00000000000018474, 297.8351940652706276 ) ) ;
#5407 = CARTESIAN_POINT ( 'NONE',  ( -49.96441683051492078, -24.99999999999981881, 542.4422122871054626 ) ) ;
#5408 = PRODUCT_DEFINITION ( 'UNKNOWN', '', #4001, #5224 ) ;
#5409 = EDGE_LOOP ( 'NONE', ( #4811, #4541, #3866, #9, #2, #3405, #4810, #4514 ) ) ;
#5410 = LINE ( 'NONE', #1644, #1022 ) ;
#5411 = APPLICATION_CONTEXT ( 'automotive_design' ) ;
#5412 = ORIENTED_EDGE ( 'NONE', *, *, #1604, .T. ) ;
#5413 = EDGE_LOOP ( 'NONE', ( #2649, #874, #2889, #1550 ) ) ;
#5414 = AXIS2_PLACEMENT_3D ( 'NONE', #180, #1830, #3495 ) ;
#5415 = CARTESIAN_POINT ( 'NONE',  ( 29.23877717791895492, -14.99999999999998579, 67.09613410133256650 ) ) ;
#5416 = DIRECTION ( 'NONE',  ( 0.000000000000000000, 0.000000000000000000, 1.000000000000000000 ) ) ;
#5417 = CARTESIAN_POINT ( 'NONE',  ( 133.9714219172562366, -21.54565493204319182, -2.000000000000001776 ) ) ;
#5418 = FACE_BOUND ( 'NONE', #3944, .T. ) ;
#5419 = CLOSED_SHELL ( 'NONE', ( #4583, #2308, #3847, #4761, #1597, #402 ) ) ;
#5420 = ORIENTED_EDGE ( 'NONE', *, *, #1917, .T. ) ;
#5421 = ORIENTED_EDGE ( 'NONE', *, *, #2685, .T. ) ;
#5422 = DIRECTION ( 'NONE',  ( -1.000000000000000000, -1.219242865862094703E-16, 0.000000000000000000 ) ) ;
#5423 = CARTESIAN_POINT ( 'NONE',  ( -349.7655555707380017, 2.222614453595284090E-15, 158.2793954369929850 ) ) ;
#5424 = DIRECTION ( 'NONE',  ( -0.09383933793885536334, 2.626968444144180070E-31, 0.9955873536034882676 ) ) ;
#5425 = EDGE_CURVE ( 'NONE', #2290, #5037, #1427, .T. ) ;
#5426 = EDGE_CURVE ( 'NONE', #1846, #4186, #1170, .T. ) ;
#5427 = DIRECTION ( 'NONE',  ( 0.09383933793885568253, -2.673190762809473730E-31, -0.9955873536034882676 ) ) ;
#5428 = EDGE_CURVE ( 'NONE', #4465, #800, #1705, .T. ) ;
#5429 = AXIS2_PLACEMENT_3D ( 'NONE', #778, #2896, #3294 ) ;
#5430 = EDGE_CURVE ( 'NONE', #2476, #5147, #3202, .T. ) ;
#5431 = CARTESIAN_POINT ( 'NONE',  ( 10.82492224058167984, 3.740497495074990297E-15, 312.2165827548582229 ) ) ;
#5432 = SHAPE_REPRESENTATION_RELATIONSHIP ( 'NONE' , 'NONE' ,  #3052, #3454 ) ;
#5433 = NEXT_ASSEMBLY_USAGE_OCCURRENCE ( 'NAUO1', ' ', ' ', #2160, #2322, $ ) ;
#5434 = NEXT_ASSEMBLY_USAGE_OCCURRENCE ( 'NAUO2', ' ', ' ', #2160, #5408, $ ) ;
#5435 = NEXT_ASSEMBLY_USAGE_OCCURRENCE ( 'NAUO3', ' ', ' ', #2160, #4505, $ ) ;
#5436 = NEXT_ASSEMBLY_USAGE_OCCURRENCE ( 'NAUO4', ' ', ' ', #2160, #377, $ ) ;
#5437 = NEXT_ASSEMBLY_USAGE_OCCURRENCE ( 'NAUO5', ' ', ' ', #2160, #3211, $ ) ;
#5438=COLOUR_RGB('Dark Blue',0.08,0.2,0.34);
#5439=FILL_AREA_STYLE_COLOUR('',#5438);
#5440=FILL_AREA_STYLE('',(#5439));
#5441=SURFACE_STYLE_FILL_AREA(#5440);
#5442=SURFACE_SIDE_STYLE('',(#5441));
#5443=SURFACE_STYLE_USAGE(.BOTH.,#5442);
#5444=PRESENTATION_STYLE_ASSIGNMENT((#5443));
#5445=COLOUR_RGB('Light Blue',0.38,0.62,0.78);
#5446=FILL_AREA_STYLE_COLOUR('',#5445);
#5447=FILL_AREA_STYLE('',(#5446));
#5448=SURFACE_STYLE_FILL_AREA(#5447);
#5449=SURFACE_SIDE_STYLE('',(#5448));
#5450=SURFACE_STYLE_USAGE(.BOTH.,#5449);
#5451=PRESENTATION_STYLE_ASSIGNMENT((#5450));
#5452=COLOUR_RGB('Sky Blue',0.24,0.69,0.87);
#5453=FILL_AREA_STYLE_COLOUR('',#5452);
#5454=FILL_AREA_STYLE('',(#5453));
#5455=SURFACE_STYLE_FILL_AREA(#5454);
#5456=SURFACE_SIDE_STYLE('',(#5455));
#5457=SURFACE_STYLE_USAGE(.BOTH.,#5456);
#5458=PRESENTATION_STYLE_ASSIGNMENT((#5457));
#5459=COLOUR_RGB('Grey',0.48,0.52,0.57);
#5460=FILL_AREA_STYLE_COLOUR('',#5459);
#5461=FILL_AREA_STYLE('',(#5460));
#5462=SURFACE_STYLE_FILL_AREA(#5461);
#5463=SURFACE_SIDE_STYLE('',(#5462));
#5464=SURFACE_STYLE_USAGE(.BOTH.,#5463);
#5465=PRESENTATION_STYLE_ASSIGNMENT((#5464));
#5466=COLOUR_RGB('Black',0.12,0.14,0.17);
#5467=FILL_AREA_STYLE_COLOUR('',#5466);
#5468=FILL_AREA_STYLE('',(#5467));
#5469=SURFACE_STYLE_FILL_AREA(#5468);
#5470=SURFACE_SIDE_STYLE('',(#5469));
#5471=SURFACE_STYLE_USAGE(.BOTH.,#5470);
#5472=PRESENTATION_STYLE_ASSIGNMENT((#5471));
#5473=COLOUR_RGB('Off White',0.89,0.88,0.83);
#5474=FILL_AREA_STYLE_COLOUR('',#5473);
#5475=FILL_AREA_STYLE('',(#5474));
#5476=SURFACE_STYLE_FILL_AREA(#5475);
#5477=SURFACE_SIDE_STYLE('',(#5476));
#5478=SURFACE_STYLE_USAGE(.BOTH.,#5477);
#5479=PRESENTATION_STYLE_ASSIGNMENT((#5478));
ENDSEC;
END-ISO-10303-21;
